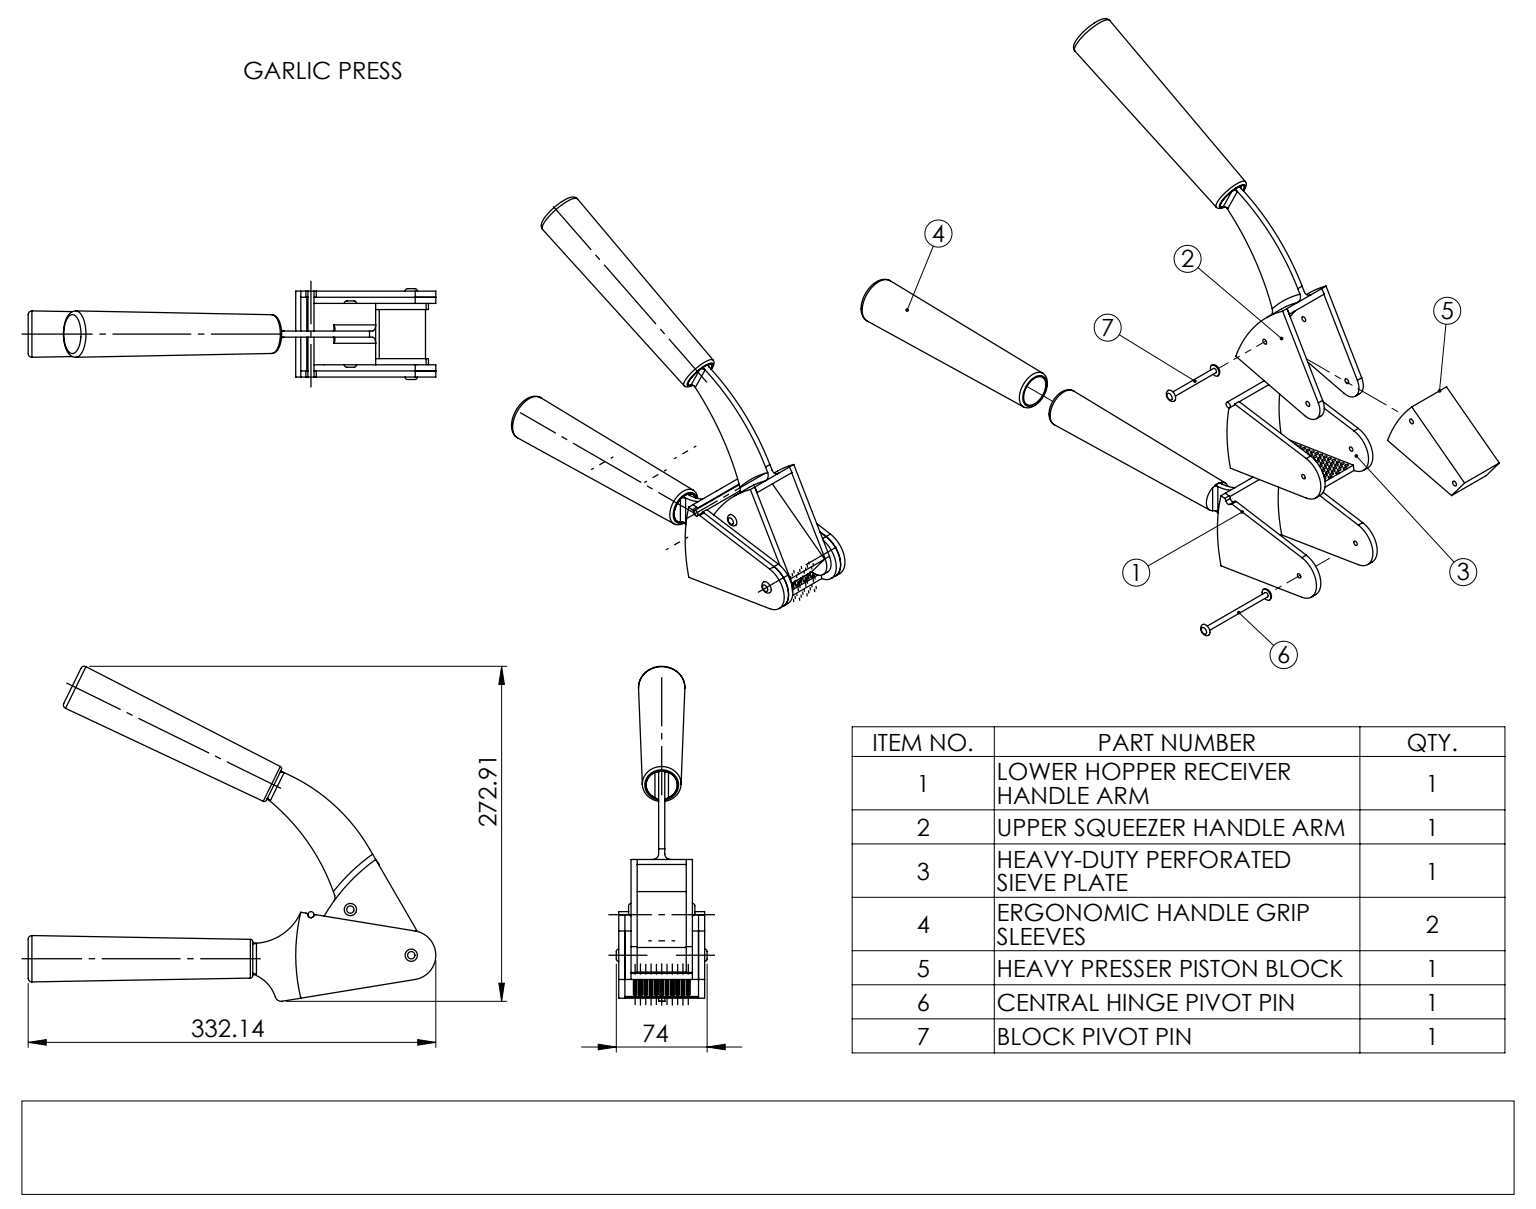
ISO-10303-21;
HEADER;
FILE_DESCRIPTION (('STEP AP214'),
    '1' );
FILE_NAME ('BR-825',
    '2026-10-02T13:02:33',
    ( '' ),
    ( '' ),
    'SwSTEP 2.0',
    'SolidWorks 2026',
    '' );
FILE_SCHEMA (( 'AUTOMOTIVE_DESIGN' ));
ENDSEC;

DATA;
#1 = DIRECTION ( 'NONE',  ( -0.9876526153536341335, -0.1566598588826327021, 0.000000000000000000 ) ) ;
#2 = VERTEX_POINT ( 'NONE', #2570 ) ;
#3 = LINE ( 'NONE', #7217, #14699 ) ;
#4 = ADVANCED_FACE ( 'NONE', ( #13839 ), #888, .F. ) ;
#5 = CARTESIAN_POINT ( 'NONE',  ( -30.20514499443620338, -82.74634522781904877, 4.330127018922213189 ) ) ;
#6 = AXIS2_PLACEMENT_3D ( 'NONE', #420, #4760, #13466 ) ;
#8 = ORIENTED_EDGE ( 'NONE', *, *, #17949, .T. ) ;
#7 = DIRECTION ( 'NONE',  ( 0.000000000000000000, 0.000000000000000000, 1.000000000000000000 ) ) ;
#9 = CIRCLE ( 'NONE', #3911, 1.500000000000000888 ) ;
#10 = ORIENTED_EDGE ( 'NONE', *, *, #1419, .F. ) ;
#11 = CYLINDRICAL_SURFACE ( 'NONE', #12678, 1.500000000000001554 ) ;
#12 = AXIS2_PLACEMENT_3D ( 'NONE', #5144, #6683, #9508 ) ;
#13 = ORIENTED_EDGE ( 'NONE', *, *, #7836, .F. ) ;
#14 = VERTEX_POINT ( 'NONE', #10991 ) ;
#15 = ORIENTED_EDGE ( 'NONE', *, *, #18047, .F. ) ;
#16 = DIRECTION ( 'NONE',  ( -0.1566598588826321192, 0.9876526153536342445, 7.798540720466730171E-17 ) ) ;
#17 = FACE_BOUND ( 'NONE', #10882, .T. ) ;
#18 = AXIS2_PLACEMENT_3D ( 'NONE', #16860, #4970, #18101 ) ;
#19 = EDGE_CURVE ( 'NONE', #12170, #1369, #18158, .T. ) ;
#20 = DIRECTION ( 'NONE',  ( -0.9876526153536341335, -0.1566598588826327021, 0.000000000000000000 ) ) ;
#21 = ORIENTED_EDGE ( 'NONE', *, *, #15181, .F. ) ;
#22 = EDGE_CURVE ( 'NONE', #3591, #12466, #3580, .T. ) ;
#23 = EDGE_CURVE ( 'NONE', #2732, #16279, #9785, .T. ) ;
#24 = EDGE_CURVE ( 'NONE', #1802, #4978, #17849, .T. ) ;
#25 = AXIS2_PLACEMENT_3D ( 'NONE', #11149, #18028, #14009 ) ;
#26 = DIRECTION ( 'NONE',  ( -0.1566598588826321192, 0.9876526153536342445, 7.798540720466730171E-17 ) ) ;
#27 = CARTESIAN_POINT ( 'NONE',  ( -56.41757431148525370, -29.19865005186066043, 17.32050807568881723 ) ) ;
#28 = DIRECTION ( 'NONE',  ( -0.1566598588826321192, 0.9876526153536342445, 7.798540720466730171E-17 ) ) ;
#29 = LINE ( 'NONE', #5530, #5145 ) ;
#30 = FACE_OUTER_BOUND ( 'NONE', #13183, .T. ) ;
#31 = AXIS2_PLACEMENT_3D ( 'NONE', #12240, #913, #6318 ) ;
#32 = DIRECTION ( 'NONE',  ( -0.1566598588826321192, 0.9876526153536342445, 7.798540720466730171E-17 ) ) ;
#33 = ORIENTED_EDGE ( 'NONE', *, *, #662, .F. ) ;
#34 = CIRCLE ( 'NONE', #6695, 1.500000000000000888 ) ;
#35 = ORIENTED_EDGE ( 'NONE', *, *, #7081, .F. ) ;
#36 = EDGE_LOOP ( 'NONE', ( #5022, #14370, #8560, #13804 ) ) ;
#37 = ORIENTED_EDGE ( 'NONE', *, *, #12771, .T. ) ;
#38 = ORIENTED_EDGE ( 'NONE', *, *, #14374, .T. ) ;
#39 = LINE ( 'NONE', #5829, #1016 ) ;
#40 = ORIENTED_EDGE ( 'NONE', *, *, #10473, .T. ) ;
#41 = DIRECTION ( 'NONE',  ( 0.000000000000000000, 0.000000000000000000, 1.000000000000000000 ) ) ;
#42 = AXIS2_PLACEMENT_3D ( 'NONE', #5371, #11127, #3921 ) ;
#43 = CARTESIAN_POINT ( 'NONE',  ( -67.24211807019732134, -88.62108993591773753, 1.443110928631665584E-14 ) ) ;
#44 = VERTEX_POINT ( 'NONE', #12516 ) ;
#45 = AXIS2_PLACEMENT_3D ( 'NONE', #1422, #5499, #1514 ) ;
#46 = CARTESIAN_POINT ( 'NONE',  ( -71.02801022084922522, -26.45362499944938506, 12.99038105676661736 ) ) ;
#47 = APPLICATION_PROTOCOL_DEFINITION ( 'draft international standard', 'automotive_design', 1998, #364 ) ;
#48 = CIRCLE ( 'NONE', #6755, 1.500000000000000000 ) ;
#49 = CARTESIAN_POINT ( 'NONE',  ( 0.000000000000000000, 0.000000000000000000, 32.00000000000000000 ) ) ;
#50 = DIRECTION ( 'NONE',  ( 0.000000000000000000, 0.000000000000000000, 1.000000000000000000 ) ) ;
#51 = EDGE_CURVE ( 'NONE', #10382, #2699, #15096, .T. ) ;
#52 = VECTOR ( 'NONE', #9149, 1000.000000000000000 ) ;
#53 = DIRECTION ( 'NONE',  ( -0.9876526153536336894, -0.1566598588826349503, 0.000000000000000000 ) ) ;
#54 = ORIENTED_EDGE ( 'NONE', *, *, #7944, .T. ) ;
#55 = EDGE_CURVE ( 'NONE', #14250, #12234, #5712, .T. ) ;
#56 = VERTEX_POINT ( 'NONE', #8559 ) ;
#57 = FACE_OUTER_BOUND ( 'NONE', #3238, .T. ) ;
#58 = CARTESIAN_POINT ( 'NONE',  ( -47.32434745236211171, -22.69378838626622397, 1.926565525561698076E-14 ) ) ;
#59 = CIRCLE ( 'NONE', #13963, 20.00000000000001066 ) ;
#60 = CARTESIAN_POINT ( 'NONE',  ( -84.16561914167408531, -33.59999999999994458, -30.00000000000000000 ) ) ;
#61 = CIRCLE ( 'NONE', #8830, 1.500000000000000444 ) ;
#62 = VERTEX_POINT ( 'NONE', #27 ) ;
#63 = LINE ( 'NONE', #14371, #9733 ) ;
#64 = ORIENTED_EDGE ( 'NONE', *, *, #598, .T. ) ;
#65 = AXIS2_PLACEMENT_3D ( 'NONE', #12198, #9374, #18037 ) ;
#66 = VECTOR ( 'NONE', #7491, 1000.000000000000000 ) ;
#67 = DIRECTION ( 'NONE',  ( -0.1566598588826321192, 0.9876526153536342445, 7.798540720466730171E-17 ) ) ;
#68 = CARTESIAN_POINT ( 'NONE',  ( -27.28182215855319015, -24.57718421482303484, -4.330127018922181215 ) ) ;
#69 = DIRECTION ( 'NONE',  ( -0.1566598588826321192, 0.9876526153536342445, 7.798540720466731404E-17 ) ) ;
#70 =( NAMED_UNIT ( * ) SI_UNIT ( $, .STERADIAN. ) SOLID_ANGLE_UNIT ( ) );
#71 = CIRCLE ( 'NONE', #9451, 3.000000000000000000 ) ;
#72 = DIRECTION ( 'NONE',  ( -0.9876526153536336894, -0.1566598588826349503, 0.000000000000000000 ) ) ;
#73 = DIRECTION ( 'NONE',  ( -0.1566598588826321192, 0.9876526153536342445, 7.798540720466731404E-17 ) ) ;
#74 = DIRECTION ( 'NONE',  ( -0.1566598588826321192, 0.9876526153536342445, 7.798540720466730171E-17 ) ) ;
#75 = CYLINDRICAL_SURFACE ( 'NONE', #18095, 1.500000000000001554 ) ;
#76 = EDGE_LOOP ( 'NONE', ( #16554, #5977 ) ) ;
#77 = CARTESIAN_POINT ( 'NONE',  ( -30.53425299135042081, -20.03057078526148516, 8.660254037844417496 ) ) ;
#78 = ADVANCED_FACE ( 'NONE', ( #8643 ), #2771, .F. ) ;
#80 = ORIENTED_EDGE ( 'NONE', *, *, #17512, .T. ) ;
#79 = CARTESIAN_POINT ( 'NONE',  ( -22.79775037928398618, -81.57139628619931671, 17.32050807568881368 ) ) ;
#81 = EDGE_CURVE ( 'NONE', #12067, #4830, #257, .T. ) ;
#82 = DIRECTION ( 'NONE',  ( 0.000000000000000000, 0.000000000000000000, 1.000000000000000000 ) ) ;
#83 = ORIENTED_EDGE ( 'NONE', *, *, #3528, .F. ) ;
#84 = CARTESIAN_POINT ( 'NONE',  ( 0.000000000000000000, 0.000000000000000000, 35.00000000000000000 ) ) ;
#85 = ADVANCED_FACE ( 'NONE', ( #5892 ), #18647, .T. ) ;
#86 = CARTESIAN_POINT ( 'NONE',  ( -89.99999999999998579, -35.00000000000001421, 100.5765140304660861 ) ) ;
#87 =( GEOMETRIC_REPRESENTATION_CONTEXT ( 3 ) GLOBAL_UNCERTAINTY_ASSIGNED_CONTEXT ( ( #8912 ) ) GLOBAL_UNIT_ASSIGNED_CONTEXT ( ( #3872, #4067, #6666 ) ) REPRESENTATION_CONTEXT ( 'NONE', 'WORKASPACE' ) );
#88 = DIRECTION ( 'NONE',  ( -0.000000000000000000, -0.000000000000000000, -1.000000000000000000 ) ) ;
#89 = CYLINDRICAL_SURFACE ( 'NONE', #17046, 1.500000000000001554 ) ;
#90 = DIRECTION ( 'NONE',  ( -0.1566598588826321192, 0.9876526153536342445, 7.798540720466730171E-17 ) ) ;
#91 = CARTESIAN_POINT ( 'NONE',  ( -66.78792677269836986, -30.84357857012828674, 21.65063509461101887 ) ) ;
#92 = CARTESIAN_POINT ( 'NONE',  ( -75.18297400320422241, -32.17518737063066681, 21.65063509461101887 ) ) ;
#93 = VERTEX_POINT ( 'NONE', #10234 ) ;
#94 = DIRECTION ( 'NONE',  ( -0.1566598588826321747, 0.9876526153536343555, 0.000000000000000000 ) ) ;
#95 = DIRECTION ( 'NONE',  ( -0.1566598588826321747, 0.9876526153536343555, 0.000000000000000000 ) ) ;
#96 = CARTESIAN_POINT ( 'NONE',  ( -127.1404785156000941, 9.613695087247878135, -2.500000000000000000 ) ) ;
#97 = ORIENTED_EDGE ( 'NONE', *, *, #2052, .T. ) ;
#98 = VERTEX_POINT ( 'NONE', #12699 ) ;
#99 = CARTESIAN_POINT ( 'NONE',  ( -129.1404785418517918, 9.649298036820672664, 2.500000000000000000 ) ) ;
#100 = AXIS2_PLACEMENT_3D ( 'NONE', #10768, #16585, #15534 ) ;
#101 = EDGE_CURVE ( 'NONE', #13042, #12109, #10138, .T. ) ;
#102 = ORIENTED_EDGE ( 'NONE', *, *, #16935, .T. ) ;
#103 = ORIENTED_EDGE ( 'NONE', *, *, #6276, .F. ) ;
#104 = DIRECTION ( 'NONE',  ( -0.9876526153536336894, -0.1566598588826349503, 0.000000000000000000 ) ) ;
#105 = FACE_BOUND ( 'NONE', #10139, .T. ) ;
#106 = ADVANCED_FACE ( 'NONE', ( #14516 ), #13086, .F. ) ;
#107 = ORIENTED_EDGE ( 'NONE', *, *, #8467, .F. ) ;
#108 = ORIENTED_EDGE ( 'NONE', *, *, #6919, .T. ) ;
#109 =( NAMED_UNIT ( * ) SI_UNIT ( $, .STERADIAN. ) SOLID_ANGLE_UNIT ( ) );
#110 = AXIS2_PLACEMENT_3D ( 'NONE', #4893, #11798, #13415 ) ;
#111 = CARTESIAN_POINT ( 'NONE',  ( 0.000000000000000000, 0.000000000000000000, 35.00000000000000000 ) ) ;
#112 = ORIENTED_EDGE ( 'NONE', *, *, #1667, .T. ) ;
#113 = VERTEX_POINT ( 'NONE', #1359 ) ;
#114 = CARTESIAN_POINT ( 'NONE',  ( -84.16561914167411373, 33.60000000000000142, -30.00000000000000000 ) ) ;
#115 = EDGE_LOOP ( 'NONE', ( #1862, #4295 ) ) ;
#116 = DIRECTION ( 'NONE',  ( -0.9723968097209879646, 0.2333333333333338921, -0.000000000000000000 ) ) ;
#118 = EDGE_CURVE ( 'NONE', #9740, #1864, #12345, .T. ) ;
#117 = LINE ( 'NONE', #3375, #307 ) ;
#119 = FACE_OUTER_BOUND ( 'NONE', #18220, .T. ) ;
#120 = FACE_BOUND ( 'NONE', #14429, .T. ) ;
#121 = DIRECTION ( 'NONE',  ( -0.1566598588826321192, 0.9876526153536342445, 7.798540720466730171E-17 ) ) ;
#122 = EDGE_LOOP ( 'NONE', ( #6243, #4264, #10759 ) ) ;
#123 = EDGE_CURVE ( 'NONE', #15608, #18110, #18554, .T. ) ;
#124 = ORIENTED_EDGE ( 'NONE', *, *, #13553, .F. ) ;
#125 = ORIENTED_EDGE ( 'NONE', *, *, #6218, .F. ) ;
#126 = CARTESIAN_POINT ( 'NONE',  ( -306.1404785418517918, -2.850701963179328668, 9.951701414186818625E-16 ) ) ;
#127 = EDGE_CURVE ( 'NONE', #15127, #18093, #8457, .T. ) ;
#128 = EDGE_CURVE ( 'NONE', #14364, #5884, #10830, .T. ) ;
#129 = ORIENTED_EDGE ( 'NONE', *, *, #2912, .F. ) ;
#130 = FACE_OUTER_BOUND ( 'NONE', #4986, .T. ) ;
#131 = EDGE_CURVE ( 'NONE', #13266, #3195, #7839, .T. ) ;
#132 = CYLINDRICAL_SURFACE ( 'NONE', #16628, 1.500000000000001554 ) ;
#133 = EDGE_LOOP ( 'NONE', ( #5269, #5864 ) ) ;
#134 = EDGE_CURVE ( 'NONE', #306, #3989, #4730, .T. ) ;
#135 = DIRECTION ( 'NONE',  ( -0.9876526153536344665, -0.1566598588826304539, 0.000000000000000000 ) ) ;
#136 = CARTESIAN_POINT ( 'NONE',  ( -54.89646037827696290, -86.66284169988483654, -12.99038105676658539 ) ) ;
#137 = DIRECTION ( 'NONE',  ( -0.1566598588826321192, 0.9876526153536342445, 7.798540720466731404E-17 ) ) ;
#138 = CARTESIAN_POINT ( 'NONE',  ( -48.02252708097939404, -27.86704125135830523, 8.660254037844417496 ) ) ;
#139 = VERTEX_POINT ( 'NONE', #14880 ) ;
#140 = ORIENTED_EDGE ( 'NONE', *, *, #2716, .F. ) ;
#141 = DIRECTION ( 'NONE',  ( -1.000000000000000000, 0.000000000000000000, 0.000000000000000000 ) ) ;
#142 = EDGE_LOOP ( 'NONE', ( #9264, #8766, #6960, #18741, #15276 ) ) ;
#143 = CARTESIAN_POINT ( 'NONE',  ( -35.67686938905902849, -25.90879301532540779, -4.330127018922181215 ) ) ;
#144 = CARTESIAN_POINT ( 'NONE',  ( -24.27922930231443743, -81.80638607452327449, 8.660254037844412167 ) ) ;
#145 = EDGE_CURVE ( 'NONE', #1457, #13070, #13868, .T. ) ;
#146 = ORIENTED_EDGE ( 'NONE', *, *, #12497, .F. ) ;
#147 = DIRECTION ( 'NONE',  ( -0.1566598588826321747, 0.9876526153536343555, 0.000000000000000000 ) ) ;
#148 = EDGE_CURVE ( 'NONE', #7107, #5722, #1632, .T. ) ;
#149 = EDGE_CURVE ( 'NONE', #14051, #4382, #6373, .T. ) ;
#150 = EDGE_CURVE ( 'NONE', #1792, #949, #14691, .T. ) ;
#151 = DIRECTION ( 'NONE',  ( -0.1566598588826321192, 0.9876526153536342445, 7.798540720466730171E-17 ) ) ;
#152 = TOROIDAL_SURFACE ( 'NONE', #18040, 3.000000000000004441, 2.000000000000000000 ) ;
#153 = LINE ( 'NONE', #5658, #5168 ) ;
#154 = CARTESIAN_POINT ( 'NONE',  ( -70.24471092643608472, -31.39188807621751209, 21.65063509461101887 ) ) ;
#155 = SHAPE_REPRESENTATION_RELATIONSHIP ( 'NONE' , 'NONE' ,  #6739, #1868 ) ;
#156 = EDGE_LOOP ( 'NONE', ( #2014, #11521, #8711, #17506 ) ) ;
#157 = CARTESIAN_POINT ( 'NONE',  ( -33.00338452973448966, -20.42222043246806251, 4.330127018922218518 ) ) ;
#158 = DIRECTION ( 'NONE',  ( -0.1566598588826321192, 0.9876526153536342445, 7.798540720466730171E-17 ) ) ;
#159 = DIRECTION ( 'NONE',  ( -0.1566598588826321192, 0.9876526153536342445, 7.798540720466730171E-17 ) ) ;
#160 = CARTESIAN_POINT ( 'NONE',  ( -18.35331361019266794, -80.86642692122747178, 4.330127018922213189 ) ) ;
#161 = ORIENTED_EDGE ( 'NONE', *, *, #2086, .F. ) ;
#162 = FACE_OUTER_BOUND ( 'NONE', #5968, .T. ) ;
#164 = ORIENTED_EDGE ( 'NONE', *, *, #5902, .T. ) ;
#163 = CARTESIAN_POINT ( 'NONE',  ( -6.047290928450125946, -21.20899724884646531, -21.65063509461098334 ) ) ;
#165 = CIRCLE ( 'NONE', #14403, 12.74754878398197633 ) ;
#166 = CARTESIAN_POINT ( 'NONE',  ( -39.91695283720987675, -21.51883944464648479, -4.330127018922180326 ) ) ;
#167 = EDGE_LOOP ( 'NONE', ( #17757, #5769 ) ) ;
#168 = CARTESIAN_POINT ( 'NONE',  ( -16.91146969734005268, -22.93225569655540141, -8.660254037844380193 ) ) ;
#169 = EDGE_CURVE ( 'NONE', #4575, #3501, #2377, .T. ) ;
#170 = DIRECTION ( 'NONE',  ( -0.9876526153536336894, -0.1566598588826349503, 0.000000000000000000 ) ) ;
#171 = FACE_OUTER_BOUND ( 'NONE', #4320, .T. ) ;
#172 = DIRECTION ( 'NONE',  ( -0.1566598588826321192, 0.9876526153536342445, 7.798540720466730171E-17 ) ) ;
#173 = CARTESIAN_POINT ( 'NONE',  ( -58.88670584986932255, -29.59029969906724133, 12.99038105676661736 ) ) ;
#174 = EDGE_CURVE ( 'NONE', #9818, #7902, #192, .T. ) ;
#175 = LINE ( 'NONE', #6157, #13878 ) ;
#176 = AXIS2_PLACEMENT_3D ( 'NONE', #2016, #3423, #9416 ) ;
#177 = ORIENTED_EDGE ( 'NONE', *, *, #17607, .F. ) ;
#178 = CARTESIAN_POINT ( 'NONE',  ( -22.79775037928398618, -81.57139628619930249, -17.32050807568878525 ) ) ;
#179 = CARTESIAN_POINT ( 'NONE',  ( -34.19539046602857724, -25.67380322700145356, 12.99038105676661736 ) ) ;
#180 = ORIENTED_EDGE ( 'NONE', *, *, #16256, .T. ) ;
#181 = ORIENTED_EDGE ( 'NONE', *, *, #3310, .F. ) ;
#182 = CARTESIAN_POINT ( 'NONE',  ( -60.36818477289978091, -29.82528948739120267, -12.99038105676658006 ) ) ;
#183 = CIRCLE ( 'NONE', #2605, 1.500000000000000888 ) ;
#184 = ORIENTED_EDGE ( 'NONE', *, *, #555, .T. ) ;
#185 = ORIENTED_EDGE ( 'NONE', *, *, #890, .F. ) ;
#186 = CARTESIAN_POINT ( 'NONE',  ( -68.55887868246516348, -26.06197535224280770, 17.32050807568882078 ) ) ;
#187 = CARTESIAN_POINT ( 'NONE',  ( -37.94164760650264867, -21.20551972688121012, -21.65063509461098334 ) ) ;
#188 = EDGE_LOOP ( 'NONE', ( #13607, #15627 ) ) ;
#189 = CARTESIAN_POINT ( 'NONE',  ( -49.01017969633304006, -28.02370111024093191, -12.99038105676658006 ) ) ;
#190 = CIRCLE ( 'NONE', #802, 42.89102435249441925 ) ;
#191 = EDGE_CURVE ( 'NONE', #13070, #8810, #6083, .T. ) ;
#192 = LINE ( 'NONE', #17673, #12969 ) ;
#193 = EDGE_LOOP ( 'NONE', ( #12370, #7151, #5297, #6845 ) ) ;
#194 =( NAMED_UNIT ( * ) PLANE_ANGLE_UNIT ( ) SI_UNIT ( $, .RADIAN. ) );
#195 = ORIENTED_EDGE ( 'NONE', *, *, #18603, .T. ) ;
#196 = CARTESIAN_POINT ( 'NONE',  ( -64.20000000000000284, 2.694222958124180951E-16, -25.00000000000000000 ) ) ;
#197 = AXIS2_PLACEMENT_3D ( 'NONE', #13789, #13899, #10956 ) ;
#199 = EDGE_CURVE ( 'NONE', #827, #16818, #10252, .T. ) ;
#198 = DIRECTION ( 'NONE',  ( 1.000000000000000000, 0.000000000000000000, -0.000000000000000000 ) ) ;
#200 = DIRECTION ( 'NONE',  ( -0.1566598588826321192, 0.9876526153536342445, 7.798540720466731404E-17 ) ) ;
#201 = ADVANCED_FACE ( 'NONE', ( #1648 ), #132, .F. ) ;
#202 = VERTEX_POINT ( 'NONE', #5909 ) ;
#203 = ORIENTED_EDGE ( 'NONE', *, *, #2611, .T. ) ;
#204 = ORIENTED_EDGE ( 'NONE', *, *, #16861, .F. ) ;
#205 = ORIENTED_EDGE ( 'NONE', *, *, #601, .T. ) ;
#206 = DIRECTION ( 'NONE',  ( -0.1566598588826321192, 0.9876526153536342445, 7.798540720466731404E-17 ) ) ;
#207 = AXIS2_PLACEMENT_3D ( 'NONE', #17977, #18347, #1736 ) ;
#208 = ORIENTED_EDGE ( 'NONE', *, *, #14608, .T. ) ;
#209 = FACE_BOUND ( 'NONE', #76, .T. ) ;
#210 = CARTESIAN_POINT ( 'NONE',  ( 10.28861223506262412, -76.32329101363113466, 8.660254037844406838 ) ) ;
#211 = VERTEX_POINT ( 'NONE', #5994 ) ;
#212 = PRESENTATION_LAYER_ASSIGNMENT (  '', '', ( #11387 ) ) ;
#213 = EDGE_LOOP ( 'NONE', ( #813, #9222, #12211, #16308 ) ) ;
#214 = CIRCLE ( 'NONE', #11085, 1.500000000000000888 ) ;
#215 = EDGE_LOOP ( 'NONE', ( #10832, #6172, #11697, #10724 ) ) ;
#216 = CIRCLE ( 'NONE', #4738, 1.500000000000000444 ) ;
#217 = DIRECTION ( 'NONE',  ( -0.9876526153536344665, -0.1566598588826304539, 0.000000000000000000 ) ) ;
#218 = CIRCLE ( 'NONE', #4461, 1.499999999999999556 ) ;
#219 = EDGE_CURVE ( 'NONE', #16637, #6756, #7426, .T. ) ;
#220 = EDGE_CURVE ( 'NONE', #5802, #9058, #10861, .T. ) ;
#221 = CARTESIAN_POINT ( 'NONE',  ( -18.39294862037050393, -23.16724548487935564, 1.869203119972154228E-14 ) ) ;
#222 = CARTESIAN_POINT ( 'NONE',  ( -10.98555400521827607, -21.99229654325962002, 12.99038105676661381 ) ) ;
#224 = EDGE_CURVE ( 'NONE', #15083, #7553, #10560, .T. ) ;
#223 = DIRECTION ( 'NONE',  ( -0.000000000000000000, -0.000000000000000000, -1.000000000000000000 ) ) ;
#225 = FACE_OUTER_BOUND ( 'NONE', #16348, .T. ) ;
#226 = ORIENTED_EDGE ( 'NONE', *, *, #15016, .F. ) ;
#227 = VERTEX_POINT ( 'NONE', #8930 ) ;
#228 = CARTESIAN_POINT ( 'NONE',  ( -19.34096622554629263, -81.02308678011010556, 1.424741226644455312E-14 ) ) ;
#229 = ORIENTED_EDGE ( 'NONE', *, *, #5595, .F. ) ;
#230 = CIRCLE ( 'NONE', #18445, 2.199999999999993516 ) ;
#231 = LINE ( 'NONE', #17611, #15362 ) ;
#232 = ORIENTED_EDGE ( 'NONE', *, *, #13411, .F. ) ;
#233 = ORIENTED_EDGE ( 'NONE', *, *, #9764, .F. ) ;
#234 = ORIENTED_EDGE ( 'NONE', *, *, #16412, .F. ) ;
#235 = CARTESIAN_POINT ( 'NONE',  ( -9.299721761247353058, -16.66238381928489787, -17.32050807568878170 ) ) ;
#236 = FACE_BOUND ( 'NONE', #6125, .T. ) ;
#237 = LINE ( 'NONE', #7306, #7511 ) ;
#238 = CARTESIAN_POINT ( 'NONE',  ( -64.77298653181324539, -88.22944028871116018, 21.65063509461101532 ) ) ;
#239 = EDGE_CURVE ( 'NONE', #10470, #12526, #9677, .T. ) ;
#240 = CIRCLE ( 'NONE', #6612, 1.500000000000000444 ) ;
#241 = VERTEX_POINT ( 'NONE', #17685 ) ;
#242 = EDGE_CURVE ( 'NONE', #4960, #1643, #5109, .T. ) ;
#243 = DIRECTION ( 'NONE',  ( -0.9876526153536336894, -0.1566598588826349503, 0.000000000000000000 ) ) ;
#244 = CARTESIAN_POINT ( 'NONE',  ( -14.40270314877813895, -80.23978748569693664, -17.32050807568878525 ) ) ;
#245 = CARTESIAN_POINT ( 'NONE',  ( -129.1404785418517918, 8.649298036820676217, 5.500000000000000000 ) ) ;
#246 = CYLINDRICAL_SURFACE ( 'NONE', #528, 2.000000000000001776 ) ;
#247 = EDGE_LOOP ( 'NONE', ( #10607, #2910 ) ) ;
#248 = EDGE_LOOP ( 'NONE', ( #11901, #15407, #18357, #803 ) ) ;
#249 = CARTESIAN_POINT ( 'NONE',  ( -41.39843176024032800, -21.75382923297043192, 4.330127018922218518 ) ) ;
#250 = CIRCLE ( 'NONE', #2017, 1.500000000000000444 ) ;
#251 = AXIS2_PLACEMENT_3D ( 'NONE', #14278, #17128, #4490 ) ;
#252 = ORIENTED_EDGE ( 'NONE', *, *, #3818, .T. ) ;
#253 = VECTOR ( 'NONE', #1467, 1000.000000000000000 ) ;
#254 = EDGE_LOOP ( 'NONE', ( #5319, #8500, #14701, #2198 ) ) ;
#255 = ORIENTED_EDGE ( 'NONE', *, *, #6970, .T. ) ;
#256 = DIRECTION ( 'NONE',  ( 0.000000000000000000, 0.000000000000000000, 1.000000000000000000 ) ) ;
#257 = CIRCLE ( 'NONE', #7250, 1.499999999999999556 ) ;
#258 = LINE ( 'NONE', #13329, #11510 ) ;
#259 = DIRECTION ( 'NONE',  ( 1.000000000000000000, 0.000000000000000000, -0.000000000000000000 ) ) ;
#260 = AXIS2_PLACEMENT_3D ( 'NONE', #1453, #14527, #297 ) ;
#261 = CARTESIAN_POINT ( 'NONE',  ( -36.62488699423482785, -83.76463431055616127, -21.65063509461098690 ) ) ;
#262 = CARTESIAN_POINT ( 'NONE',  ( -41.39843176024032800, -21.75382923297042836, -4.330127018922180326 ) ) ;
#263 = CIRCLE ( 'NONE', #6336, 2.200000000000000178 ) ;
#264 = DIRECTION ( 'NONE',  ( -0.9876526153536336894, -0.1566598588826349503, 0.000000000000000000 ) ) ;
#265 = CARTESIAN_POINT ( 'NONE',  ( -26.78799585087635649, -24.49885428538171794, -8.660254037844380193 ) ) ;
#266 = FACE_OUTER_BOUND ( 'NONE', #3188, .T. ) ;
#267 = ORIENTED_EDGE ( 'NONE', *, *, #13623, .F. ) ;
#269 = EDGE_LOOP ( 'NONE', ( #9815, #12862, #15948, #5626 ) ) ;
#268 = DIRECTION ( 'NONE',  ( -0.9876526153536336894, -0.1566598588826349503, 0.000000000000000000 ) ) ;
#270 = EDGE_CURVE ( 'NONE', #17286, #16790, #6357, .T. ) ;
#271 = AXIS2_PLACEMENT_3D ( 'NONE', #15102, #6588, #11007 ) ;
#272 = VERTEX_POINT ( 'NONE', #11653 ) ;
#273 = EDGE_CURVE ( 'NONE', #17252, #3975, #18174, .T. ) ;
#274 = CARTESIAN_POINT ( 'NONE',  ( -6.047290928450125946, -21.20899724884646531, 21.65063509461101177 ) ) ;
#275 = VECTOR ( 'NONE', #8347, 1000.000000000000000 ) ;
#276 = ORIENTED_EDGE ( 'NONE', *, *, #13888, .T. ) ;
#277 = ORIENTED_EDGE ( 'NONE', *, *, #10855, .F. ) ;
#278 = FACE_OUTER_BOUND ( 'NONE', #17914, .T. ) ;
#279 = CIRCLE ( 'NONE', #11460, 1.500000000000000444 ) ;
#280 = EDGE_CURVE ( 'NONE', #14450, #6414, #16167, .T. ) ;
#281 = VECTOR ( 'NONE', #15110, 1000.000000000000000 ) ;
#282 = CIRCLE ( 'NONE', #10852, 1.500000000000000000 ) ;
#283 = DIRECTION ( 'NONE',  ( -0.9876526153536341335, -0.1566598588826327021, 0.000000000000000000 ) ) ;
#284 = CARTESIAN_POINT ( 'NONE',  ( 2.000000000000000000, 0.000000000000000000, 30.00000000000000000 ) ) ;
#285 = CARTESIAN_POINT ( 'NONE',  ( -13.25033222266188560, -17.28902325481542235, 4.330127018922214965 ) ) ;
#286 = AXIS2_PLACEMENT_3D ( 'NONE', #9882, #15657, #10154 ) ;
#287 = AXIS2_PLACEMENT_3D ( 'NONE', #9251, #13887, #9450 ) ;
#288 = DIRECTION ( 'NONE',  ( 0.9826218788918642533, 0.1856185419698762884, -0.000000000000000000 ) ) ;
#289 = AXIS2_PLACEMENT_3D ( 'NONE', #791, #6676, #10995 ) ;
#290 = ORIENTED_EDGE ( 'NONE', *, *, #11265, .T. ) ;
#291 = FACE_BOUND ( 'NONE', #9868, .T. ) ;
#292 = AXIS2_PLACEMENT_3D ( 'NONE', #3529, #12534, #16843 ) ;
#293 = DIRECTION ( 'NONE',  ( -1.000000000000000000, 0.000000000000000000, 0.000000000000000000 ) ) ;
#294 = VERTEX_POINT ( 'NONE', #7445 ) ;
#295 = DIRECTION ( 'NONE',  ( -0.9876526153536341335, -0.1566598588826327021, 0.000000000000000000 ) ) ;
#296 = VECTOR ( 'NONE', #9069, 1000.000000000000000 ) ;
#297 = DIRECTION ( 'NONE',  ( 0.000000000000000000, 0.000000000000000000, 1.000000000000000000 ) ) ;
#298 = ORIENTED_EDGE ( 'NONE', *, *, #1505, .F. ) ;
#299 = VERTEX_POINT ( 'NONE', #6020 ) ;
#300 = ORIENTED_EDGE ( 'NONE', *, *, #13362, .F. ) ;
#301 = AXIS2_PLACEMENT_3D ( 'NONE', #1034, #11223, #5560 ) ;
#302 = ORIENTED_EDGE ( 'NONE', *, *, #6850, .F. ) ;
#303 = DIRECTION ( 'NONE',  ( -0.9876526153536336894, -0.1566598588826349503, 0.000000000000000000 ) ) ;
#304 = EDGE_CURVE ( 'NONE', #7962, #8290, #17617, .T. ) ;
#305 = ORIENTED_EDGE ( 'NONE', *, *, #9387, .T. ) ;
#306 = VERTEX_POINT ( 'NONE', #6126 ) ;
#307 = VECTOR ( 'NONE', #16481, 1000.000000000000000 ) ;
#308 = FACE_BOUND ( 'NONE', #13049, .T. ) ;
#309 = DIRECTION ( 'NONE',  ( -0.9876526153536336894, -0.1566598588826349503, 0.000000000000000000 ) ) ;
#310 = VECTOR ( 'NONE', #14810, 1000.000000000000000 ) ;
#311 = VERTEX_POINT ( 'NONE', #14829 ) ;
#312 = CARTESIAN_POINT ( 'NONE',  ( -23.33121169713865584, -23.95054477929251036, -8.660254037844380193 ) ) ;
#313 = VECTOR ( 'NONE', #867, 1000.000000000000000 ) ;
#314 = EDGE_LOOP ( 'NONE', ( #6630, #11469 ) ) ;
#315 = EDGE_CURVE ( 'NONE', #5884, #5893, #1848, .T. ) ;
#316 = EDGE_CURVE ( 'NONE', #12986, #12973, #2391, .T. ) ;
#317 = EDGE_LOOP ( 'NONE', ( #16039, #7700, #562, #13733 ) ) ;
#318 = AXIS2_PLACEMENT_3D ( 'NONE', #5866, #8616, #8694 ) ;
#319 = DIRECTION ( 'NONE',  ( 0.000000000000000000, 0.000000000000000000, 1.000000000000000000 ) ) ;
#320 = DIRECTION ( 'NONE',  ( -0.1566598588826321192, 0.9876526153536342445, 7.798540720466730171E-17 ) ) ;
#322 = CARTESIAN_POINT ( 'NONE',  ( -13.45468554360235203, -22.38394619046619383, 1.869203119972154228E-14 ) ) ;
#321 = AXIS2_PLACEMENT_3D ( 'NONE', #1598, #12854, #13040 ) ;
#323 = DIRECTION ( 'NONE',  ( -0.1566598588826321192, 0.9876526153536342445, 7.798540720466731404E-17 ) ) ;
#324 = CARTESIAN_POINT ( 'NONE',  ( -6.995308533625909320, -79.06483854407721878, 21.65063509461100821 ) ) ;
#325 = LINE ( 'NONE', #9139, #5689 ) ;
#326 = ORIENTED_EDGE ( 'NONE', *, *, #13082, .F. ) ;
#327 = ORIENTED_EDGE ( 'NONE', *, *, #12450, .F. ) ;
#328 = LINE ( 'NONE', #4668, #9322 ) ;
#329 = AXIS2_PLACEMENT_3D ( 'NONE', #4692, #16469, #16269 ) ;
#330 = DIRECTION ( 'NONE',  ( -0.1566598588826321192, 0.9876526153536342445, 7.798540720466730171E-17 ) ) ;
#331 = DIRECTION ( 'NONE',  ( -0.1566598588826321192, 0.9876526153536342445, 7.798540720466730171E-17 ) ) ;
#332 = CIRCLE ( 'NONE', #3341, 1.500000000000000888 ) ;
#333 = ADVANCED_FACE ( 'NONE', ( #10729 ), #15383, .F. ) ;
#334 = VERTEX_POINT ( 'NONE', #16930 ) ;
#335 = CARTESIAN_POINT ( 'NONE',  ( -75.18297400320422241, -32.17518737063066681, 21.65063509461101887 ) ) ;
#336 = CIRCLE ( 'NONE', #16374, 1.500000000000000888 ) ;
#338 = FACE_BOUND ( 'NONE', #5848, .T. ) ;
#337 = AXIS2_PLACEMENT_3D ( 'NONE', #9442, #15216, #13774 ) ;
#339 = EDGE_CURVE ( 'NONE', #7418, #9571, #3618, .T. ) ;
#340 = DIRECTION ( 'NONE',  ( 0.000000000000000000, 0.000000000000000000, 1.000000000000000000 ) ) ;
#341 = CIRCLE ( 'NONE', #12123, 1.500000000000001332 ) ;
#342 = DIRECTION ( 'NONE',  ( -0.1566598588826321192, 0.9876526153536342445, 7.798540720466731404E-17 ) ) ;
#343 = DIRECTION ( 'NONE',  ( -0.1566598588826321192, 0.9876526153536342445, 7.798540720466730171E-17 ) ) ;
#344 = VERTEX_POINT ( 'NONE', #5255 ) ;
#345 = DIRECTION ( 'NONE',  ( -0.1566598588826321747, 0.9876526153536343555, 0.000000000000000000 ) ) ;
#346 = CARTESIAN_POINT ( 'NONE',  ( -45.34904222165486942, -22.38046866850094929, -17.32050807568878170 ) ) ;
#347 = AXIS2_PLACEMENT_3D ( 'NONE', #6635, #963, #6737 ) ;
#348 = VECTOR ( 'NONE', #6882, 1000.000000000000000 ) ;
#349 = FACE_OUTER_BOUND ( 'NONE', #8068, .T. ) ;
#350 = LINE ( 'NONE', #15811, #2031 ) ;
#351 = EDGE_LOOP ( 'NONE', ( #7291, #2729, #13644, #16148 ) ) ;
#352 = CARTESIAN_POINT ( 'NONE',  ( -45.01993422474065198, -85.09624311105852712, 4.330127018922213189 ) ) ;
#353 = EDGE_CURVE ( 'NONE', #8550, #12053, #18503, .T. ) ;
#354 = ORIENTED_EDGE ( 'NONE', *, *, #5419, .T. ) ;
#355 = CIRCLE ( 'NONE', #13059, 2.000000000000000000 ) ;
#356 = VERTEX_POINT ( 'NONE', #16529 ) ;
#357 = EDGE_CURVE ( 'NONE', #4379, #18393, #1509, .T. ) ;
#358 = EDGE_CURVE ( 'NONE', #1477, #15259, #8155, .T. ) ;
#359 = EDGE_CURVE ( 'NONE', #9050, #9141, #4270, .T. ) ;
#360 = EDGE_LOOP ( 'NONE', ( #2874, #17765 ) ) ;
#361 = DIRECTION ( 'NONE',  ( 0.000000000000000000, 0.000000000000000000, 1.000000000000000000 ) ) ;
#362 = EDGE_CURVE ( 'NONE', #1820, #10566, #9051, .T. ) ;
#363 = AXIS2_PLACEMENT_3D ( 'NONE', #14211, #2358, #12673 ) ;
#364 = APPLICATION_CONTEXT ( 'automotive_design' ) ;
#365 = DIRECTION ( 'NONE',  ( -0.1566598588826321192, 0.9876526153536342445, 7.798540720466730171E-17 ) ) ;
#366 = ORIENTED_EDGE ( 'NONE', *, *, #8931, .T. ) ;
#367 = CARTESIAN_POINT ( 'NONE',  ( -48.80582637539254875, -22.92877817459017464, 17.32050807568882078 ) ) ;
#368 = CARTESIAN_POINT ( 'NONE',  ( -66.25446545484369665, -88.46443007703511796, -12.99038105676658539 ) ) ;
#369 = DIRECTION ( 'NONE',  ( -0.9876526153536336894, -0.1566598588826349503, 0.000000000000000000 ) ) ;
#370 = VERTEX_POINT ( 'NONE', #11385 ) ;
#371 = AXIS2_PLACEMENT_3D ( 'NONE', #10848, #743, #7570 ) ;
#372 = CARTESIAN_POINT ( 'NONE',  ( -46.50141314777110324, -85.33123289938248490, 4.330127018922213189 ) ) ;
#373 = ORIENTED_EDGE ( 'NONE', *, *, #11541, .F. ) ;
#374 = DIRECTION ( 'NONE',  ( 1.000000000000000000, 0.000000000000000000, 0.000000000000000000 ) ) ;
#375 = AXIS2_PLACEMENT_3D ( 'NONE', #5395, #11058, #12194 ) ;
#376 = DIRECTION ( 'NONE',  ( -0.9876526153536341335, -0.1566598588826327021, 0.000000000000000000 ) ) ;
#377 = EDGE_LOOP ( 'NONE', ( #5700, #15642 ) ) ;
#379 = ORIENTED_EDGE ( 'NONE', *, *, #9515, .T. ) ;
#378 = DIRECTION ( 'NONE',  ( -0.9876526153536341335, -0.1566598588826327021, 0.000000000000000000 ) ) ;
#380 = CIRCLE ( 'NONE', #16419, 13.78215425775057668 ) ;
#381 = ORIENTED_EDGE ( 'NONE', *, *, #387, .F. ) ;
#382 = DIRECTION ( 'NONE',  ( 0.000000000000000000, 0.000000000000000000, 1.000000000000000000 ) ) ;
#383 = ORIENTED_EDGE ( 'NONE', *, *, #18100, .F. ) ;
#384 = VERTEX_POINT ( 'NONE', #4086 ) ;
#385 = EDGE_LOOP ( 'NONE', ( #16397, #10275 ) ) ;
#386 = DIRECTION ( 'NONE',  ( -0.9876526153536341335, -0.1566598588826327021, 0.000000000000000000 ) ) ;
#387 = EDGE_CURVE ( 'NONE', #11399, #16710, #13584, .T. ) ;
#388 = STYLED_ITEM ( 'NONE', ( #17094 ), #8708 ) ;
#389 = ORIENTED_EDGE ( 'NONE', *, *, #13835, .T. ) ;
#390 = CARTESIAN_POINT ( 'NONE',  ( -48.97054468615517919, -85.72288254658904805, 8.660254037844412167 ) ) ;
#391 = ORIENTED_EDGE ( 'NONE', *, *, #358, .T. ) ;
#392 = CYLINDRICAL_SURFACE ( 'NONE', #15221, 1.500000000000001554 ) ;
#393 = ORIENTED_EDGE ( 'NONE', *, *, #4749, .F. ) ;
#394 = EDGE_CURVE ( 'NONE', #17063, #537, #14514, .T. ) ;
#395 = LINE ( 'NONE', #17952, #3848 ) ;
#396 = ORIENTED_EDGE ( 'NONE', *, *, #516, .F. ) ;
#397 = ORIENTED_EDGE ( 'NONE', *, *, #14939, .F. ) ;
#398 = AXIS2_PLACEMENT_3D ( 'NONE', #6831, #12574, #2548 ) ;
#399 = DIRECTION ( 'NONE',  ( -0.9876526153536336894, -0.1566598588826350336, 0.000000000000000000 ) ) ;
#400 = FACE_OUTER_BOUND ( 'NONE', #2830, .T. ) ;
#401 = ORIENTED_EDGE ( 'NONE', *, *, #13050, .T. ) ;
#402 = ORIENTED_EDGE ( 'NONE', *, *, #11892, .F. ) ;
#403 = VERTEX_POINT ( 'NONE', #17028 ) ;
#404 = ORIENTED_EDGE ( 'NONE', *, *, #8014, .T. ) ;
#405 = VERTEX_POINT ( 'NONE', #2589 ) ;
#406 = ORIENTED_EDGE ( 'NONE', *, *, #492, .F. ) ;
#407 = CARTESIAN_POINT ( 'NONE',  ( -21.81009776393036503, -81.41473642731666871, -21.65063509461098690 ) ) ;
#408 = ORIENTED_EDGE ( 'NONE', *, *, #6164, .F. ) ;
#409 = ORIENTED_EDGE ( 'NONE', *, *, #15155, .F. ) ;
#410 = FACE_BOUND ( 'NONE', #1885, .T. ) ;
#411 = VERTEX_POINT ( 'NONE', #18575 ) ;
#412 = CARTESIAN_POINT ( 'NONE',  ( -44.03228160938703439, -84.93958325217590755, 8.660254037844412167 ) ) ;
#413 = ORIENTED_EDGE ( 'NONE', *, *, #12861, .T. ) ;
#414 = ADVANCED_FACE ( 'NONE', ( #17211 ), #2684, .T. ) ;
#415 = ORIENTED_EDGE ( 'NONE', *, *, #13647, .F. ) ;
#416 = FACE_BOUND ( 'NONE', #8311, .T. ) ;
#417 = DIRECTION ( 'NONE',  ( 1.000000000000000000, 0.000000000000000000, 0.000000000000000000 ) ) ;
#418 = ADVANCED_FACE ( 'NONE', ( #10070 ), #1375, .F. ) ;
#419 = CARTESIAN_POINT ( 'NONE',  ( -46.50141314777111745, -85.33123289938247069, -21.65063509461098690 ) ) ;
#420 = CARTESIAN_POINT ( 'NONE',  ( -75.18297400320422241, -32.17518737063066681, 4.330127018922217630 ) ) ;
#421 = PLANE ( 'NONE',  #6625 ) ;
#422 = DIRECTION ( 'NONE',  ( -0.1566598588826321192, 0.9876526153536342445, 7.798540720466731404E-17 ) ) ;
#423 = DIRECTION ( 'NONE',  ( -0.9876526153536336894, -0.1566598588826349503, 0.000000000000000000 ) ) ;
#424 = ORIENTED_EDGE ( 'NONE', *, *, #224, .F. ) ;
#425 = EDGE_LOOP ( 'NONE', ( #6614, #11556 ) ) ;
#426 = TOROIDAL_SURFACE ( 'NONE', #13412, 155.0000000000000284, 5.000000000000000000 ) ;
#427 = CARTESIAN_POINT ( 'NONE',  ( -51.97313754239394257, -28.49368068688882971, -21.65063509461098334 ) ) ;
#428 = DIRECTION ( 'NONE',  ( -0.1566598588826321192, 0.9876526153536342445, 7.798540720466730171E-17 ) ) ;
#429 = ORIENTED_EDGE ( 'NONE', *, *, #3774, .F. ) ;
#430 = CARTESIAN_POINT ( 'NONE',  ( -349.0394899966146909, 23.59157312255261729, 2.567204941047426911E-15 ) ) ;
#431 = DIRECTION ( 'NONE',  ( -0.1566598588826321192, 0.9876526153536342445, 7.798540720466730171E-17 ) ) ;
#432 = DIRECTION ( 'NONE',  ( -0.1566598588826321192, 0.9876526153536342445, 7.798540720466731404E-17 ) ) ;
#433 = FACE_OUTER_BOUND ( 'NONE', #8720, .T. ) ;
#434 = EDGE_CURVE ( 'NONE', #14223, #211, #7251, .T. ) ;
#435 = CARTESIAN_POINT ( 'NONE',  ( -1.109027851681966492, -20.42569795443330349, 12.99038105676661026 ) ) ;
#436 = FACE_OUTER_BOUND ( 'NONE', #14679, .T. ) ;
#437 = CARTESIAN_POINT ( 'NONE',  ( -38.10636591726525069, -83.99962409888011905, 21.65063509461101532 ) ) ;
#438 = DIRECTION ( 'NONE',  ( 1.000000000000000000, 0.000000000000000000, 0.000000000000000000 ) ) ;
#439 = ORIENTED_EDGE ( 'NONE', *, *, #9830, .F. ) ;
#440 = ORIENTED_EDGE ( 'NONE', *, *, #10556, .F. ) ;
#441 = DIRECTION ( 'NONE',  ( -0.1566598588826321192, 0.9876526153536342445, 7.798540720466730171E-17 ) ) ;
#442 = VERTEX_POINT ( 'NONE', #9802 ) ;
#443 = ORIENTED_EDGE ( 'NONE', *, *, #4057, .T. ) ;
#444 = EDGE_CURVE ( 'NONE', #18320, #13724, #15774, .T. ) ;
#445 = ORIENTED_EDGE ( 'NONE', *, *, #17707, .F. ) ;
#446 = CIRCLE ( 'NONE', #10419, 1.500000000000000444 ) ;
#447 = DIRECTION ( 'NONE',  ( 0.000000000000000000, 0.000000000000000000, -1.000000000000000000 ) ) ;
#448 = ORIENTED_EDGE ( 'NONE', *, *, #11230, .F. ) ;
#449 = DIRECTION ( 'NONE',  ( -0.1566598588826321192, 0.9876526153536342445, 7.798540720466730171E-17 ) ) ;
#450 = VERTEX_POINT ( 'NONE', #8374 ) ;
#451 = DIRECTION ( 'NONE',  ( -0.1566598588826321747, 0.9876526153536343555, 0.000000000000000000 ) ) ;
#452 = DIRECTION ( 'NONE',  ( -0.1566598588826321747, 0.9876526153536343555, 0.000000000000000000 ) ) ;
#453 = DIRECTION ( 'NONE',  ( -0.9876526153536341335, -0.1566598588826327021, 0.000000000000000000 ) ) ;
#454 = PRODUCT ( 'Central Hinge Pivot Pin', 'Central Hinge Pivot Pin', '', ( #9983 ) ) ;
#455 = CARTESIAN_POINT ( 'NONE',  ( -37.61253960958843834, -83.92129416943879505, 1.443110928631665584E-14 ) ) ;
#456 = ORIENTED_EDGE ( 'NONE', *, *, #5446, .T. ) ;
#457 = FACE_OUTER_BOUND ( 'NONE', #12580, .T. ) ;
#458 = FACE_BOUND ( 'NONE', #12232, .T. ) ;
#459 = ADVANCED_FACE ( 'NONE', ( #14152 ), #2791, .F. ) ;
#460 = DIRECTION ( 'NONE',  ( -0.1566598588826321192, 0.9876526153536342445, 7.798540720466730171E-17 ) ) ;
#461 = ORIENTED_EDGE ( 'NONE', *, *, #12663, .T. ) ;
#462 = DIRECTION ( 'NONE',  ( -0.1566598588826321192, 0.9876526153536342445, 7.798540720466730171E-17 ) ) ;
#463 = EDGE_CURVE ( 'NONE', #931, #3364, #13273, .T. ) ;
#464 = VECTOR ( 'NONE', #8302, 1000.000000000000000 ) ;
#466 = ORIENTED_EDGE ( 'NONE', *, *, #9742, .F. ) ;
#465 = FACE_OUTER_BOUND ( 'NONE', #17810, .T. ) ;
#467 = EDGE_CURVE ( 'NONE', #9397, #7759, #14260, .T. ) ;
#468 = LINE ( 'NONE', #1619, #12903 ) ;
#469 = EDGE_LOOP ( 'NONE', ( #9333, #3211, #5541, #13498 ) ) ;
#470 = ORIENTED_EDGE ( 'NONE', *, *, #17168, .T. ) ;
#471 = ORIENTED_EDGE ( 'NONE', *, *, #13823, .T. ) ;
#472 = CARTESIAN_POINT ( 'NONE',  ( -38.10636591726526490, -83.99962409888010484, -12.99038105676658539 ) ) ;
#473 = CYLINDRICAL_SURFACE ( 'NONE', #18582, 1.500000000000001554 ) ;
#474 = ORIENTED_EDGE ( 'NONE', *, *, #16472, .T. ) ;
#475 = CYLINDRICAL_SURFACE ( 'NONE', #1700, 1.500000000000000888 ) ;
#476 = CARTESIAN_POINT ( 'NONE',  ( 3.000000000000000000, 4.898587196589412829E-16, -37.00000000000000711 ) ) ;
#477 = AXIS2_PLACEMENT_3D ( 'NONE', #13662, #13565, #10447 ) ;
#478 = DIRECTION ( 'NONE',  ( 0.000000000000000000, 0.000000000000000000, 1.000000000000000000 ) ) ;
#479 = DIRECTION ( 'NONE',  ( -1.000000000000000000, 0.000000000000000000, 0.000000000000000000 ) ) ;
#480 = LINE ( 'NONE', #6273, #9392 ) ;
#481 = CARTESIAN_POINT ( 'NONE',  ( -131.1404785418517918, -2.850701963179328668, -13.78215425775057490 ) ) ;
#482 = VERTEX_POINT ( 'NONE', #1195 ) ;
#483 = FACE_BOUND ( 'NONE', #13486, .T. ) ;
#484 = EDGE_CURVE ( 'NONE', #14364, #13704, #1564, .T. ) ;
#485 = ORIENTED_EDGE ( 'NONE', *, *, #9618, .T. ) ;
#486 = VECTOR ( 'NONE', #9487, 1000.000000000000000 ) ;
#487 = DIRECTION ( 'NONE',  ( -0.9876526153536341335, -0.1566598588826327021, 0.000000000000000000 ) ) ;
#489 = EDGE_CURVE ( 'NONE', #18416, #1139, #6043, .T. ) ;
#488 = DIRECTION ( 'NONE',  ( -0.9876526153536341335, -0.1566598588826327021, 0.000000000000000000 ) ) ;
#490 = CIRCLE ( 'NONE', #15932, 13.78215425775057668 ) ;
#491 = VERTEX_POINT ( 'NONE', #2863 ) ;
#492 = EDGE_CURVE ( 'NONE', #15556, #14764, #2100, .T. ) ;
#493 = EDGE_LOOP ( 'NONE', ( #4032, #9284, #18031, #15546 ) ) ;
#494 = ORIENTED_EDGE ( 'NONE', *, *, #2458, .T. ) ;
#495 = VERTEX_POINT ( 'NONE', #13004 ) ;
#496 = CARTESIAN_POINT ( 'NONE',  ( -174.0670050711101737, 56.28339404658832024, -2.500000000000000000 ) ) ;
#497 = EDGE_LOOP ( 'NONE', ( #2948, #10572, #17851, #2071 ) ) ;
#498 = FACE_BOUND ( 'NONE', #17308, .T. ) ;
#499 = AXIS2_PLACEMENT_3D ( 'NONE', #13270, #3318, #9014 ) ;
#500 = CYLINDRICAL_SURFACE ( 'NONE', #18608, 1.500000000000001554 ) ;
#501 = ORIENTED_EDGE ( 'NONE', *, *, #11049, .F. ) ;
#502 = VECTOR ( 'NONE', #15322, 1000.000000000000000 ) ;
#503 = ORIENTED_EDGE ( 'NONE', *, *, #3380, .F. ) ;
#504 = DIRECTION ( 'NONE',  ( -0.9876526153536341335, -0.1566598588826327021, 0.000000000000000000 ) ) ;
#505 = ORIENTED_EDGE ( 'NONE', *, *, #6048, .T. ) ;
#506 = LINE ( 'NONE', #700, #9084 ) ;
#507 = CARTESIAN_POINT ( 'NONE',  ( -42.38608437559395270, -21.91048909185306925, 8.660254037844417496 ) ) ;
#508 = DIRECTION ( 'NONE',  ( 1.438274729681541867E-16, 6.252920376642369977E-17, -1.000000000000000000 ) ) ;
#509 = DIRECTION ( 'NONE',  ( 0.000000000000000000, 0.000000000000000000, 1.000000000000000000 ) ) ;
#510 = ORIENTED_EDGE ( 'NONE', *, *, #9686, .F. ) ;
#511 = EDGE_LOOP ( 'NONE', ( #3706, #485 ) ) ;
#512 = CARTESIAN_POINT ( 'NONE',  ( 5.481473465377026066, -12.88229205725314586, -19.99999999999999645 ) ) ;
#513 = AXIS2_PLACEMENT_3D ( 'NONE', #14412, #1535, #9778 ) ;
#514 = CARTESIAN_POINT ( 'NONE',  ( -129.1404785418517918, -2.850701963179328668, 9.951701414186818625E-16 ) ) ;
#515 = DIRECTION ( 'NONE',  ( -0.9876526153536336894, -0.1566598588826349503, 0.000000000000000000 ) ) ;
#516 = EDGE_CURVE ( 'NONE', #370, #16376, #2953, .T. ) ;
#517 = DIRECTION ( 'NONE',  ( 0.000000000000000000, 0.000000000000000000, 1.000000000000000000 ) ) ;
#518 = VERTEX_POINT ( 'NONE', #6943 ) ;
#519 = EDGE_CURVE ( 'NONE', #14468, #5881, #4054, .T. ) ;
#520 = VECTOR ( 'NONE', #6791, 1000.000000000000000 ) ;
#521 = ORIENTED_EDGE ( 'NONE', *, *, #3170, .T. ) ;
#522 = DIRECTION ( 'NONE',  ( -0.000000000000000000, -0.000000000000000000, -1.000000000000000000 ) ) ;
#523 = AXIS2_PLACEMENT_3D ( 'NONE', #1578, #2969, #8674 ) ;
#524 = DIRECTION ( 'NONE',  ( -0.1566598588826321747, 0.9876526153536343555, 0.000000000000000000 ) ) ;
#525 = ORIENTED_EDGE ( 'NONE', *, *, #14996, .F. ) ;
#526 = EDGE_CURVE ( 'NONE', #6605, #14798, #15112, .T. ) ;
#527 = CIRCLE ( 'NONE', #10191, 1.500000000000000888 ) ;
#528 = AXIS2_PLACEMENT_3D ( 'NONE', #2893, #8689, #14567 ) ;
#529 = DIRECTION ( 'NONE',  ( -0.1566598588826321192, 0.9876526153536342445, 7.798540720466731404E-17 ) ) ;
#530 = FACE_BOUND ( 'NONE', #4136, .T. ) ;
#531 = EDGE_LOOP ( 'NONE', ( #10532, #13578 ) ) ;
#532 = DIRECTION ( 'NONE',  ( -0.1566598588826321192, 0.9876526153536342445, 7.798540720466731404E-17 ) ) ;
#533 = DIRECTION ( 'NONE',  ( -0.9876526153536341335, -0.1566598588826327021, 0.000000000000000000 ) ) ;
#534 =( GEOMETRIC_REPRESENTATION_CONTEXT ( 3 ) GLOBAL_UNCERTAINTY_ASSIGNED_CONTEXT ( ( #9804 ) ) GLOBAL_UNIT_ASSIGNED_CONTEXT ( ( #13864, #16748, #10928 ) ) REPRESENTATION_CONTEXT ( 'NONE', 'WORKASPACE' ) );
#535 = VECTOR ( 'NONE', #11000, 1000.000000000000000 ) ;
#536 = FACE_OUTER_BOUND ( 'NONE', #6098, .T. ) ;
#537 = VERTEX_POINT ( 'NONE', #4535 ) ;
#538 = DIRECTION ( 'NONE',  ( -0.1566598588826321192, 0.9876526153536342445, 7.798540720466731404E-17 ) ) ;
#539 = ORIENTED_EDGE ( 'NONE', *, *, #13629, .T. ) ;
#540 = AXIS2_PLACEMENT_3D ( 'NONE', #14197, #7021, #18420 ) ;
#541 = ORIENTED_EDGE ( 'NONE', *, *, #18462, .T. ) ;
#542 = ORIENTED_EDGE ( 'NONE', *, *, #10730, .T. ) ;
#543 = EDGE_CURVE ( 'NONE', #4382, #4160, #12054, .T. ) ;
#544 = DIRECTION ( 'NONE',  ( -0.9876526153536344665, -0.1566598588826304539, 0.000000000000000000 ) ) ;
#545 = CARTESIAN_POINT ( 'NONE',  ( -57.20087360589841552, -24.26038697509253694, -8.660254037844380193 ) ) ;
#546 = AXIS2_PLACEMENT_3D ( 'NONE', #4997, #10776, #10699 ) ;
#547 = DIRECTION ( 'NONE',  ( -0.1566598588826321192, 0.9876526153536342445, 7.798540720466730171E-17 ) ) ;
#548 = DIRECTION ( 'NONE',  ( -0.1566598588826321192, 0.9876526153536342445, 7.798540720466731404E-17 ) ) ;
#549 = ORIENTED_EDGE ( 'NONE', *, *, #6994, .F. ) ;
#550 = CARTESIAN_POINT ( 'NONE',  ( -26.74836084069850983, -82.19803572172985184, 21.65063509461101532 ) ) ;
#551 = FILL_AREA_STYLE_COLOUR ( '', #12034 ) ;
#552 = ADVANCED_FACE ( 'NONE', ( #6251 ), #11983, .T. ) ;
#553 = AXIS2_PLACEMENT_3D ( 'NONE', #8026, #3657, #13790 ) ;
#554 = DIRECTION ( 'NONE',  ( -0.1566598588826321192, 0.9876526153536342445, 7.798540720466730171E-17 ) ) ;
#555 = EDGE_CURVE ( 'NONE', #8251, #1903, #12013, .T. ) ;
#556 = CARTESIAN_POINT ( 'NONE',  ( -16.87183468716221313, -80.63143713290354242, 12.99038105676661203 ) ) ;
#557 = AXIS2_PLACEMENT_3D ( 'NONE', #12003, #12293, #13716 ) ;
#558 = LINE ( 'NONE', #16393, #11124 ) ;
#559 = VECTOR ( 'NONE', #18084, 1000.000000000000000 ) ;
#560 = CARTESIAN_POINT ( 'NONE',  ( -43.86756329862440396, -22.14547888017701283, 8.660254037844417496 ) ) ;
#562 = ORIENTED_EDGE ( 'NONE', *, *, #1186, .T. ) ;
#561 = CARTESIAN_POINT ( 'NONE',  ( -42.55080268635658314, -84.70459346385194976, 1.443110928631665584E-14 ) ) ;
#563 = FACE_OUTER_BOUND ( 'NONE', #9796, .T. ) ;
#564 = EDGE_CURVE ( 'NONE', #10544, #13205, #12684, .T. ) ;
#565 = ORIENTED_EDGE ( 'NONE', *, *, #12861, .F. ) ;
#566 = EDGE_LOOP ( 'NONE', ( #4430, #255 ) ) ;
#567 = DIRECTION ( 'NONE',  ( -0.1566598588826321747, 0.9876526153536343555, 0.000000000000000000 ) ) ;
#568 = ADVANCED_FACE ( 'NONE', ( #7048 ), #12876, .F. ) ;
#569 = CIRCLE ( 'NONE', #2365, 150.0000000000000000 ) ;
#570 = CARTESIAN_POINT ( 'NONE',  ( -73.70149508017377116, -31.94019758230671258, -4.330127018922181215 ) ) ;
#571 = VECTOR ( 'NONE', #10120, 1000.000000000000000 ) ;
#572 = EDGE_CURVE ( 'NONE', #12438, #2916, #15328, .T. ) ;
#573 = ORIENTED_EDGE ( 'NONE', *, *, #1192, .T. ) ;
#574 = CARTESIAN_POINT ( 'NONE',  ( -2.200000000000000178, 0.000000000000000000, 25.00000000000000000 ) ) ;
#575 = CIRCLE ( 'NONE', #15701, 2.200000000000000622 ) ;
#576 = ORIENTED_EDGE ( 'NONE', *, *, #17660, .F. ) ;
#577 = CARTESIAN_POINT ( 'NONE',  ( -50.49165861936347000, -28.25869089856487903, 21.65063509461101887 ) ) ;
#578 = CYLINDRICAL_SURFACE ( 'NONE', #1583, 1.500000000000001554 ) ;
#579 = ADVANCED_FACE ( 'NONE', ( #13708 ), #5677, .F. ) ;
#580 = UNCERTAINTY_MEASURE_WITH_UNIT (LENGTH_MEASURE( 1.000000000000000082E-05 ), #14853, 'distance_accuracy_value', 'NONE');
#581 = DIRECTION ( 'NONE',  ( -0.1566598588826321747, 0.9876526153536343555, 0.000000000000000000 ) ) ;
#582 = FACE_OUTER_BOUND ( 'NONE', #8107, .T. ) ;
#583 = CARTESIAN_POINT ( 'NONE',  ( -6.830590222863280658, -16.27073417207831696, 4.330127018922214965 ) ) ;
#584 = VERTEX_POINT ( 'NONE', #8328 ) ;
#585 = CARTESIAN_POINT ( 'NONE',  ( -52.92115514756972061, -86.34952198211959740, -4.330127018922185655 ) ) ;
#586 = ORIENTED_EDGE ( 'NONE', *, *, #12943, .T. ) ;
#587 = FACE_OUTER_BOUND ( 'NONE', #13970, .T. ) ;
#588 = CIRCLE ( 'NONE', #9042, 1.500000000000000888 ) ;
#589 = AXIS2_PLACEMENT_3D ( 'NONE', #10009, #16176, #5934 ) ;
#590 = CARTESIAN_POINT ( 'NONE',  ( -49.79347899074619477, -23.08543803347279422, -21.65063509461098334 ) ) ;
#591 = CIRCLE ( 'NONE', #11158, 1.500000000000001332 ) ;
#592 = VERTEX_POINT ( 'NONE', #4242 ) ;
#593 = ORIENTED_EDGE ( 'NONE', *, *, #12961, .T. ) ;
#594 = ORIENTED_EDGE ( 'NONE', *, *, #8585, .F. ) ;
#595 = CARTESIAN_POINT ( 'NONE',  ( -42.38608437559395270, -21.91048909185306570, 1.926565525561698076E-14 ) ) ;
#596 = EDGE_CURVE ( 'NONE', #7360, #1643, #10020, .T. ) ;
#597 = FACE_BOUND ( 'NONE', #11849, .T. ) ;
#598 = EDGE_CURVE ( 'NONE', #9513, #6519, #16338, .T. ) ;
#599 = AXIS2_PLACEMENT_3D ( 'NONE', #9609, #16835, #3523 ) ;
#600 = ADVANCED_FACE ( 'NONE', ( #10108 ), #4133, .F. ) ;
#601 = EDGE_CURVE ( 'NONE', #8134, #12438, #12857, .T. ) ;
#602 = CARTESIAN_POINT ( 'NONE',  ( -20.86208015875458344, -23.55889513208593655, 4.330127018922217630 ) ) ;
#603 = VECTOR ( 'NONE', #5115, 1000.000000000000000 ) ;
#604 = ORIENTED_EDGE ( 'NONE', *, *, #11122, .T. ) ;
#605 = VECTOR ( 'NONE', #12622, 1000.000000000000000 ) ;
#606 = AXIS2_PLACEMENT_3D ( 'NONE', #12503, #16894, #9679 ) ;
#607 = VECTOR ( 'NONE', #8603, 1000.000000000000000 ) ;
#608 = ORIENTED_EDGE ( 'NONE', *, *, #18557, .T. ) ;
#609 = FACE_BOUND ( 'NONE', #5299, .T. ) ;
#610 = VERTEX_POINT ( 'NONE', #13044 ) ;
#611 = FACE_OUTER_BOUND ( 'NONE', #2046, .T. ) ;
#612 = ORIENTED_EDGE ( 'NONE', *, *, #8796, .F. ) ;
#613 = DIRECTION ( 'NONE',  ( -0.9876526153536336894, -0.1566598588826349503, 0.000000000000000000 ) ) ;
#614 = FACE_OUTER_BOUND ( 'NONE', #5842, .T. ) ;
#615 = AXIS2_PLACEMENT_3D ( 'NONE', #12181, #13417, #453 ) ;
#616 = DIRECTION ( 'NONE',  ( -0.1566598588826321192, 0.9876526153536342445, 7.798540720466730171E-17 ) ) ;
#617 = DIRECTION ( 'NONE',  ( -0.9876526153536336894, -0.1566598588826349503, 0.000000000000000000 ) ) ;
#618 = ORIENTED_EDGE ( 'NONE', *, *, #8953, .T. ) ;
#619 = ORIENTED_EDGE ( 'NONE', *, *, #10277, .T. ) ;
#620 = CARTESIAN_POINT ( 'NONE',  ( -0.5755665338273089349, -78.04654946134009208, -21.65063509461098690 ) ) ;
#621 = AXIS2_PLACEMENT_3D ( 'NONE', #894, #5241, #613 ) ;
#622 = CARTESIAN_POINT ( 'NONE',  ( 0.000000000000000000, 0.000000000000000000, 24.99999999999999289 ) ) ;
#623 = CYLINDRICAL_SURFACE ( 'NONE', #6256, 1.500000000000001554 ) ;
#624 = ORIENTED_EDGE ( 'NONE', *, *, #17746, .T. ) ;
#625 = FACE_OUTER_BOUND ( 'NONE', #8989, .T. ) ;
#626 = VERTEX_POINT ( 'NONE', #5942 ) ;
#627 = VECTOR ( 'NONE', #13045, 1000.000000000000000 ) ;
#628 = FACE_OUTER_BOUND ( 'NONE', #2003, .T. ) ;
#629 = CIRCLE ( 'NONE', #16060, 1.500000000000000888 ) ;
#630 = DIRECTION ( 'NONE',  ( -0.9876526153536341335, -0.1566598588826330907, 0.000000000000000000 ) ) ;
#631 = EDGE_CURVE ( 'NONE', #4650, #2328, #2045, .T. ) ;
#632 = EDGE_LOOP ( 'NONE', ( #12628, #11654, #16155, #8883 ) ) ;
#633 = CIRCLE ( 'NONE', #2130, 1.500000000000000000 ) ;
#634 = ADVANCED_FACE ( 'NONE', ( #824 ), #15404, .T. ) ;
#635 = DIRECTION ( 'NONE',  ( 0.000000000000000000, 0.000000000000000000, 1.000000000000000000 ) ) ;
#636 = VECTOR ( 'NONE', #10205, 1000.000000000000000 ) ;
#637 = CYLINDRICAL_SURFACE ( 'NONE', #5402, 1.500000000000001554 ) ;
#638 = DIRECTION ( 'NONE',  ( 0.000000000000000000, 0.000000000000000000, 1.000000000000000000 ) ) ;
#639 = EDGE_LOOP ( 'NONE', ( #12804, #15222 ) ) ;
#640 = EDGE_LOOP ( 'NONE', ( #4206, #1912, #17476, #10777 ) ) ;
#641 = DIRECTION ( 'NONE',  ( -0.1566598588826321192, 0.9876526153536342445, 7.798540720466730171E-17 ) ) ;
#642 = EDGE_LOOP ( 'NONE', ( #576, #3191 ) ) ;
#643 = AXIS2_PLACEMENT_3D ( 'NONE', #1751, #7726, #1586 ) ;
#644 = CARTESIAN_POINT ( 'NONE',  ( -33.00338452973448966, -20.42222043246806606, 12.99038105676661736 ) ) ;
#645 = ORIENTED_EDGE ( 'NONE', *, *, #717, .T. ) ;
#646 = DIRECTION ( 'NONE',  ( -0.1566598588826321747, 0.9876526153536343555, 0.000000000000000000 ) ) ;
#647 = CARTESIAN_POINT ( 'NONE',  ( 10.28861223506262412, -76.32329101363113466, -8.660254037844389075 ) ) ;
#648 = AXIS2_PLACEMENT_3D ( 'NONE', #10093, #14649, #17614 ) ;
#649 = CYLINDRICAL_SURFACE ( 'NONE', #9079, 1.500000000000001554 ) ;
#650 = CARTESIAN_POINT ( 'NONE',  ( 55.85952145814821534, 6.938893903907228378E-15, -30.00000000000000000 ) ) ;
#651 = DIRECTION ( 'NONE',  ( 0.000000000000000000, 0.000000000000000000, 1.000000000000000000 ) ) ;
#652 = DIRECTION ( 'NONE',  ( -0.1566598588826321747, 0.9876526153536343555, 0.000000000000000000 ) ) ;
#653 = EDGE_CURVE ( 'NONE', #16941, #893, #3016, .T. ) ;
#654 = AXIS2_PLACEMENT_3D ( 'NONE', #15823, #11614, #7302 ) ;
#655 = ADVANCED_FACE ( 'NONE', ( #2425 ), #15585, .F. ) ;
#656 = DIRECTION ( 'NONE',  ( -0.1566598588826321747, 0.9876526153536343555, 0.000000000000000000 ) ) ;
#657 = DIRECTION ( 'NONE',  ( -0.9876526153536336894, -0.1566598588826349503, 0.000000000000000000 ) ) ;
#658 = FACE_BOUND ( 'NONE', #11920, .T. ) ;
#659 = CARTESIAN_POINT ( 'NONE',  ( -84.16561914167408531, -33.59999999999994458, -30.00000000000000000 ) ) ;
#660 = TOROIDAL_SURFACE ( 'NONE', #5229, 12.83663829214476060, 3.000000000000000000 ) ;
#661 = FACE_OUTER_BOUND ( 'NONE', #1913, .T. ) ;
#662 = EDGE_CURVE ( 'NONE', #6476, #14356, #11311, .T. ) ;
#663 = CARTESIAN_POINT ( 'NONE',  ( -33.20773785067495254, -25.51714336811882688, -17.32050807568878170 ) ) ;
#665 = ORIENTED_EDGE ( 'NONE', *, *, #1714, .F. ) ;
#664 = CARTESIAN_POINT ( 'NONE',  ( -49.79347899074619477, -23.08543803347279777, -12.99038105676658006 ) ) ;
#666 = AXIS2_PLACEMENT_3D ( 'NONE', #9517, #14150, #12441 ) ;
#667 = CARTESIAN_POINT ( 'NONE',  ( -64.77298653181324539, -88.22944028871116018, 4.330127018922213189 ) ) ;
#668 = EDGE_LOOP ( 'NONE', ( #10359, #125, #12635, #15355, #1976 ) ) ;
#669 = EDGE_CURVE ( 'NONE', #3382, #9105, #9816, .T. ) ;
#670 = VECTOR ( 'NONE', #1243, 1000.000000000000000 ) ;
#671 = PLANE ( 'NONE',  #9426 ) ;
#672 = ORIENTED_EDGE ( 'NONE', *, *, #2828, .F. ) ;
#673 = CIRCLE ( 'NONE', #17636, 1.500000000000001332 ) ;
#674 = DIRECTION ( 'NONE',  ( -0.9876526153536341335, -0.1566598588826327021, 0.000000000000000000 ) ) ;
#675 = CARTESIAN_POINT ( 'NONE',  ( -70.24471092643608472, -31.39188807621751209, -4.330127018922181215 ) ) ;
#676 = CARTESIAN_POINT ( 'NONE',  ( 0.000000000000000000, 0.000000000000000000, 35.00000000000000000 ) ) ;
#677 = CARTESIAN_POINT ( 'NONE',  ( -21.84973277410820458, -23.71555499096855613, 8.660254037844417496 ) ) ;
#678 = CARTESIAN_POINT ( 'NONE',  ( -129.1404785418517918, -2.850701963179328668, 9.951701414186818625E-16 ) ) ;
#679 = CARTESIAN_POINT ( 'NONE',  ( -70.00000000000000000, 44.99999999999999289, -19.99999999999999645 ) ) ;
#680 = ORIENTED_EDGE ( 'NONE', *, *, #12590, .F. ) ;
#681 =( LENGTH_UNIT ( ) NAMED_UNIT ( * ) SI_UNIT ( .MILLI., .METRE. ) );
#682 = DIRECTION ( 'NONE',  ( -0.5989998693185457634, -0.8007491221077704946, 0.000000000000000000 ) ) ;
#683 = EDGE_CURVE ( 'NONE', #5280, #3602, #11594, .T. ) ;
#684 = DIRECTION ( 'NONE',  ( -0.1566598588826321192, 0.9876526153536342445, 7.798540720466730171E-17 ) ) ;
#685 = CARTESIAN_POINT ( 'NONE',  ( -84.16561914167408531, -33.59999999999994458, 30.00000000000000000 ) ) ;
#686 = AXIS2_PLACEMENT_3D ( 'NONE', #16566, #452, #6525 ) ;
#687 = ORIENTED_EDGE ( 'NONE', *, *, #7447, .F. ) ;
#688 = EDGE_LOOP ( 'NONE', ( #15524, #11717, #9471, #1813 ) ) ;
#689 = EDGE_LOOP ( 'NONE', ( #1640, #7060 ) ) ;
#690 = EDGE_CURVE ( 'NONE', #16087, #855, #10278, .T. ) ;
#691 = ORIENTED_EDGE ( 'NONE', *, *, #6782, .T. ) ;
#692 = EDGE_LOOP ( 'NONE', ( #8385, #4021 ) ) ;
#693 = DIRECTION ( 'NONE',  ( -1.000000000000000000, 0.000000000000000000, 0.000000000000000000 ) ) ;
#694 = FACE_BOUND ( 'NONE', #15508, .T. ) ;
#695 = CYLINDRICAL_SURFACE ( 'NONE', #15624, 1.500000000000001554 ) ;
#696 = DIRECTION ( 'NONE',  ( 0.000000000000000000, 0.000000000000000000, 1.000000000000000000 ) ) ;
#697 = VERTEX_POINT ( 'NONE', #8248 ) ;
#698 = PRESENTATION_LAYER_ASSIGNMENT (  '', '', ( #18286 ) ) ;
#699 = DIRECTION ( 'NONE',  ( -0.1566598588826321192, 0.9876526153536342445, 7.798540720466731404E-17 ) ) ;
#700 = CARTESIAN_POINT ( 'NONE',  ( -28.22983976372896109, -82.43302551005379541, 12.99038105676661203 ) ) ;
#701 = CARTESIAN_POINT ( 'NONE',  ( -79.30363509306917535, 32.43333333333333002, 25.00000000000002132 ) ) ;
#702 = CYLINDRICAL_SURFACE ( 'NONE', #4184, 1.500000000000001554 ) ;
#703 = CARTESIAN_POINT ( 'NONE',  ( 11.59211860341528144, 6.314490184041265053, -130.3485206753969976 ) ) ;
#704 = EDGE_CURVE ( 'NONE', #8986, #862, #12070, .T. ) ;
#705 = EDGE_LOOP ( 'NONE', ( #18497, #13074 ) ) ;
#706 = ORIENTED_EDGE ( 'NONE', *, *, #10496, .T. ) ;
#707 = DIRECTION ( 'NONE',  ( -0.1566598588826321192, 0.9876526153536342445, 7.798540720466731404E-17 ) ) ;
#708 = EDGE_CURVE ( 'NONE', #13151, #10116, #6664, .T. ) ;
#709 = DIRECTION ( 'NONE',  ( -0.1566598588826321192, 0.9876526153536342445, 7.798540720466730171E-17 ) ) ;
#710 = ORIENTED_EDGE ( 'NONE', *, *, #11771, .F. ) ;
#711 = CARTESIAN_POINT ( 'NONE',  ( -48.97054468615517919, -85.72288254658906226, 17.32050807568881368 ) ) ;
#712 = EDGE_CURVE ( 'NONE', #4620, #15439, #5093, .T. ) ;
#713 = CARTESIAN_POINT ( 'NONE',  ( -4.565812005419673802, -20.97400746052251108, 12.99038105676661026 ) ) ;
#714 = ORIENTED_EDGE ( 'NONE', *, *, #10708, .T. ) ;
#715 = DIRECTION ( 'NONE',  ( 0.9868632313631133801, 0.1615579233078775490, 0.000000000000000000 ) ) ;
#716 = DIRECTION ( 'NONE',  ( -2.735665993912342121E-16, -0.000000000000000000, -1.000000000000000000 ) ) ;
#717 = EDGE_CURVE ( 'NONE', #8478, #7247, #7561, .T. ) ;
#718 = CARTESIAN_POINT ( 'NONE',  ( -174.0586467429681363, 56.10169251196822415, -3.278196957010492962 ) ) ;
#719 = VERTEX_POINT ( 'NONE', #12471 ) ;
#720 = FACE_BOUND ( 'NONE', #3866, .T. ) ;
#721 = CARTESIAN_POINT ( 'NONE',  ( -2.096680467035594297, -20.58235781331593017, -8.660254037844383745 ) ) ;
#722 = CARTESIAN_POINT ( 'NONE',  ( -46.50141314777108903, -85.33123289938248490, 21.65063509461101532 ) ) ;
#723 = CARTESIAN_POINT ( 'NONE',  ( -30.73860631229088725, -25.12549372091224598, 21.65063509461101887 ) ) ;
#724 = CYLINDRICAL_SURFACE ( 'NONE', #1811, 1.500000000000001554 ) ;
#725 = CARTESIAN_POINT ( 'NONE',  ( -8.516422466834198346, -21.60064689605303911, -17.32050807568878170 ) ) ;
#726 = CARTESIAN_POINT ( 'NONE',  ( -77.65210554158829837, -32.56683701783724416, -8.660254037844380193 ) ) ;
#727 = EDGE_CURVE ( 'NONE', #16068, #9239, #3604, .T. ) ;
#728 = DIRECTION ( 'NONE',  ( -0.1566598588826321192, 0.9876526153536342445, 7.798540720466731404E-17 ) ) ;
#729 = ADVANCED_FACE ( 'NONE', ( #13640 ), #2185, .F. ) ;
#730 = VERTEX_POINT ( 'NONE', #6878 ) ;
#731 = ORIENTED_EDGE ( 'NONE', *, *, #2510, .T. ) ;
#732 = CARTESIAN_POINT ( 'NONE',  ( 0.000000000000000000, 0.000000000000000000, -35.00000000000000000 ) ) ;
#733 = EDGE_LOOP ( 'NONE', ( #1309, #17633, #9167, #16624 ) ) ;
#734 = CYLINDRICAL_SURFACE ( 'NONE', #16067, 1.500000000000001554 ) ;
#735 = ORIENTED_EDGE ( 'NONE', *, *, #17861, .T. ) ;
#736 = PRODUCT_RELATED_PRODUCT_CATEGORY ( 'part', '', ( #775 ) ) ;
#737 = ORIENTED_EDGE ( 'NONE', *, *, #9685, .F. ) ;
#738 = EDGE_CURVE ( 'NONE', #5480, #5362, #12722, .T. ) ;
#739 = CARTESIAN_POINT ( 'NONE',  ( 3.231158466157545206, -19.73726462726228092, -35.00000000000000000 ) ) ;
#740 = DIRECTION ( 'NONE',  ( -0.9876526153536341335, -0.1566598588826327021, 0.000000000000000000 ) ) ;
#741 = CARTESIAN_POINT ( 'NONE',  ( -72.71384246482016067, -31.78353772342409300, 8.660254037844417496 ) ) ;
#742 = DIRECTION ( 'NONE',  ( 0.000000000000000000, 0.000000000000000000, 1.000000000000000000 ) ) ;
#743 = DIRECTION ( 'NONE',  ( -0.1566598588826321192, 0.9876526153536342445, 7.798540720466731404E-17 ) ) ;
#744 =( LENGTH_UNIT ( ) NAMED_UNIT ( * ) SI_UNIT ( .MILLI., .METRE. ) );
#745 = DIRECTION ( 'NONE',  ( -0.1566598588826321192, 0.9876526153536342445, 7.798540720466730171E-17 ) ) ;
#746 = CARTESIAN_POINT ( 'NONE',  ( -306.0881213225399051, -2.850701963179326448, -15.83618137761393463 ) ) ;
#747 = CARTESIAN_POINT ( 'NONE',  ( -56.91140061916207316, -29.27697998130197732, 21.65063509461101887 ) ) ;
#748 = LINE ( 'NONE', #7752, #16988 ) ;
#750 = ORIENTED_EDGE ( 'NONE', *, *, #11331, .T. ) ;
#749 = DIRECTION ( 'NONE',  ( 0.000000000000000000, 0.000000000000000000, 1.000000000000000000 ) ) ;
#751 = DIRECTION ( 'NONE',  ( 1.000000000000000000, 0.000000000000000000, 0.000000000000000000 ) ) ;
#752 = VECTOR ( 'NONE', #5936, 1000.000000000000000 ) ;
#753 = VERTEX_POINT ( 'NONE', #12822 ) ;
#754 = ADVANCED_FACE ( 'NONE', ( #2793 ), #7079, .F. ) ;
#755 = VERTEX_POINT ( 'NONE', #15859 ) ;
#756 = ORIENTED_EDGE ( 'NONE', *, *, #631, .F. ) ;
#757 = EDGE_CURVE ( 'NONE', #18512, #8290, #1358, .T. ) ;
#758 = CARTESIAN_POINT ( 'NONE',  ( 6.831828081324923474, -76.87160051972034580, 8.660254037844406838 ) ) ;
#759 = ORIENTED_EDGE ( 'NONE', *, *, #8356, .F. ) ;
#760 = DIRECTION ( 'NONE',  ( -0.9876526153536336894, -0.1566598588826349503, 0.000000000000000000 ) ) ;
#761 = ADVANCED_FACE ( 'NONE', ( #14689 ), #17671, .F. ) ;
#762 = DIRECTION ( 'NONE',  ( -0.9876526153536341335, -0.1566598588826327021, 0.000000000000000000 ) ) ;
#763 = ORIENTED_EDGE ( 'NONE', *, *, #17578, .T. ) ;
#764 = FACE_OUTER_BOUND ( 'NONE', #7194, .T. ) ;
#765 = CARTESIAN_POINT ( 'NONE',  ( -128.8626752476364175, -14.87423233749613694, -4.224609204322598011 ) ) ;
#766 = DIRECTION ( 'NONE',  ( -0.000000000000000000, -0.000000000000000000, -1.000000000000000000 ) ) ;
#767 = CIRCLE ( 'NONE', #14675, 1.499999999999999556 ) ;
#768 = CARTESIAN_POINT ( 'NONE',  ( -127.1354840320379225, 9.580137489138413898, -2.662644313562638754 ) ) ;
#769 = DIRECTION ( 'NONE',  ( -0.000000000000000000, -0.000000000000000000, -1.000000000000000000 ) ) ;
#770 = ORIENTED_EDGE ( 'NONE', *, *, #8506, .F. ) ;
#771 = DIRECTION ( 'NONE',  ( 0.000000000000000000, 0.000000000000000000, 1.000000000000000000 ) ) ;
#772 = CARTESIAN_POINT ( 'NONE',  ( -43.86756329862441817, -22.14547888017700217, -17.32050807568878170 ) ) ;
#773 = DIRECTION ( 'NONE',  ( -0.9876526153536341335, -0.1566598588826327021, 0.000000000000000000 ) ) ;
#774 = CARTESIAN_POINT ( 'NONE',  ( -40.08167114797250719, -84.31294381664535820, -4.330127018922185655 ) ) ;
#775 = PRODUCT ( 'BR-825', 'BR-825', '', ( #7281 ) ) ;
#776 = EDGE_LOOP ( 'NONE', ( #9787, #14436, #16293, #12999 ) ) ;
#777 = VERTEX_POINT ( 'NONE', #10233 ) ;
#778 = EDGE_LOOP ( 'NONE', ( #10197, #3952, #17970, #7335 ) ) ;
#779 = EDGE_LOOP ( 'NONE', ( #18617, #8741 ) ) ;
#780 = CARTESIAN_POINT ( 'NONE',  ( 73.09088021254186174, 1.387778780781445676E-14, 25.00000000000000000 ) ) ;
#781 = AXIS2_PLACEMENT_3D ( 'NONE', #9710, #793, #3786 ) ;
#782 = FACE_BOUND ( 'NONE', #531, .T. ) ;
#783 = EDGE_CURVE ( 'NONE', #1828, #11020, #12691, .T. ) ;
#784 = SURFACE_SIDE_STYLE ('',( #16717 ) ) ;
#785 = CIRCLE ( 'NONE', #5003, 1.499999999999999556 ) ;
#786 = CARTESIAN_POINT ( 'NONE',  ( -32.50955822205765600, -20.34389050302674562, -8.660254037844380193 ) ) ;
#787 = EDGE_CURVE ( 'NONE', #17205, #5608, #12280, .T. ) ;
#788 = FACE_BOUND ( 'NONE', #3592, .T. ) ;
#789 = CARTESIAN_POINT ( 'NONE',  ( -131.1055737289773617, -2.850701963179328668, 9.951701414186818625E-16 ) ) ;
#790 = AXIS2_PLACEMENT_3D ( 'NONE', #5797, #17364, #11534 ) ;
#791 = CARTESIAN_POINT ( 'NONE',  ( -70.00000000000000000, 44.99999999999999289, 2.500000000000000000 ) ) ;
#792 = CARTESIAN_POINT ( 'NONE',  ( -29.05277406831996245, -19.79558099693754158, 17.32050807568882078 ) ) ;
#793 = DIRECTION ( 'NONE',  ( -0.1566598588826321747, 0.9876526153536343555, 0.000000000000000000 ) ) ;
#794 = VERTEX_POINT ( 'NONE', #15247 ) ;
#795 = VERTEX_POINT ( 'NONE', #14107 ) ;
#796 = CARTESIAN_POINT ( 'NONE',  ( -40.57549745564934085, -84.39127374608669641, 1.424741226644455312E-14 ) ) ;
#797 = ORIENTED_EDGE ( 'NONE', *, *, #18408, .F. ) ;
#798 = DIRECTION ( 'NONE',  ( -0.1566598588826321192, 0.9876526153536342445, 7.798540720466730171E-17 ) ) ;
#799 = EDGE_LOOP ( 'NONE', ( #13422, #7345, #16257, #5142 ) ) ;
#800 = ORIENTED_EDGE ( 'NONE', *, *, #2006, .T. ) ;
#801 = DIRECTION ( 'NONE',  ( -0.9876526153536336894, -0.1566598588826350336, 0.000000000000000000 ) ) ;
#802 = AXIS2_PLACEMENT_3D ( 'NONE', #11740, #14986, #10707 ) ;
#803 = ORIENTED_EDGE ( 'NONE', *, *, #16114, .T. ) ;
#804 = CARTESIAN_POINT ( 'NONE',  ( -126.1404785418517918, -15.29729532696464922, 2.500000000000000000 ) ) ;
#805 = ORIENTED_EDGE ( 'NONE', *, *, #9038, .T. ) ;
#806 = AXIS2_PLACEMENT_3D ( 'NONE', #11891, #3185, #17730 ) ;
#807 = EDGE_CURVE ( 'NONE', #4830, #12067, #9970, .T. ) ;
#808 = CARTESIAN_POINT ( 'NONE',  ( -9.299721761247353058, -16.66238381928489787, 8.660254037844413944 ) ) ;
#809 = ADVANCED_FACE ( 'NONE', ( #14209 ), #3858, .F. ) ;
#810 = CARTESIAN_POINT ( 'NONE',  ( -48.02252708097940825, -27.86704125135830523, 1.869203119972154228E-14 ) ) ;
#811 = SHAPE_DEFINITION_REPRESENTATION ( #14086, #15677 ) ;
#812 = EDGE_CURVE ( 'NONE', #4040, #5969, #7036, .T. ) ;
#813 = ORIENTED_EDGE ( 'NONE', *, *, #339, .F. ) ;
#814 = CIRCLE ( 'NONE', #2022, 1.499999999999999556 ) ;
#815 = CARTESIAN_POINT ( 'NONE',  ( -22.34355908178503114, -23.79388492040988012, -21.65063509461098334 ) ) ;
#816 = DIRECTION ( 'NONE',  ( 0.000000000000000000, 0.000000000000000000, 1.000000000000000000 ) ) ;
#817 = CARTESIAN_POINT ( 'NONE',  ( -47.98289207080156160, -85.56622268770642847, 12.99038105676661203 ) ) ;
#818 = FACE_OUTER_BOUND ( 'NONE', #1173, .T. ) ;
#819 = ORIENTED_EDGE ( 'NONE', *, *, #8066, .F. ) ;
#820 = ORIENTED_EDGE ( 'NONE', *, *, #55, .F. ) ;
#821 = FACE_OUTER_BOUND ( 'NONE', #16486, .T. ) ;
#822 = COLOUR_RGB ( '', 0.09019608, 0.27058824, 0.51372549) ;
#823 = EDGE_LOOP ( 'NONE', ( #1463, #16116, #18789, #5628 ) ) ;
#824 = FACE_OUTER_BOUND ( 'NONE', #12213, .T. ) ;
#825 = CARTESIAN_POINT ( 'NONE',  ( -40.57549745564932664, -84.39127374608669641, 8.660254037844412167 ) ) ;
#826 = ORIENTED_EDGE ( 'NONE', *, *, #17274, .F. ) ;
#827 = VERTEX_POINT ( 'NONE', #5596 ) ;
#828 = ORIENTED_EDGE ( 'NONE', *, *, #3619, .F. ) ;
#829 = CIRCLE ( 'NONE', #17492, 1.500000000000000000 ) ;
#830 = CIRCLE ( 'NONE', #16252, 2.200000000000007283 ) ;
#831 = CYLINDRICAL_SURFACE ( 'NONE', #12076, 1.500000000000000666 ) ;
#832 = CARTESIAN_POINT ( 'NONE',  ( -51.27495791377664602, -23.32042782179673779, -21.65063509461097979 ) ) ;
#833 = EDGE_CURVE ( 'NONE', #4754, #3060, #17278, .T. ) ;
#834 = ADVANCED_FACE ( 'NONE', ( #14585 ), #14490, .F. ) ;
#835 = DIRECTION ( 'NONE',  ( -0.1566598588826321192, 0.9876526153536342445, 7.798540720466730171E-17 ) ) ;
#836 = CARTESIAN_POINT ( 'NONE',  ( -346.6567719130321166, 10.97801148527007697, 9.951701414186830458E-16 ) ) ;
#837 = AXIS2_PLACEMENT_3D ( 'NONE', #2306, #16934, #3803 ) ;
#838 = ORIENTED_EDGE ( 'NONE', *, *, #18207, .F. ) ;
#839 = DIRECTION ( 'NONE',  ( -0.1566598588826321192, 0.9876526153536342445, 7.798540720466730171E-17 ) ) ;
#840 = AXIS2_PLACEMENT_3D ( 'NONE', #8135, #16786, #5089 ) ;
#841 = DIRECTION ( 'NONE',  ( -0.9876526153536341335, -0.1566598588826327021, 0.000000000000000000 ) ) ;
#842 = FACE_OUTER_BOUND ( 'NONE', #11073, .T. ) ;
#843 = VECTOR ( 'NONE', #10454, 1000.000000000000000 ) ;
#844 = DIRECTION ( 'NONE',  ( -0.000000000000000000, -0.000000000000000000, -1.000000000000000000 ) ) ;
#845 = ORIENTED_EDGE ( 'NONE', *, *, #9764, .T. ) ;
#846 = DIRECTION ( 'NONE',  ( 0.000000000000000000, -1.000000000000000000, 0.000000000000000000 ) ) ;
#847 = CARTESIAN_POINT ( 'NONE',  ( -42.87991068327079347, -21.98881902129437194, -12.99038105676658006 ) ) ;
#849 = EDGE_LOOP ( 'NONE', ( #13453, #13783, #15744, #11573 ) ) ;
#848 = DIRECTION ( 'NONE',  ( -0.1566598588826321192, 0.9876526153536342445, 7.798540720466731404E-17 ) ) ;
#850 = ORIENTED_EDGE ( 'NONE', *, *, #10300, .T. ) ;
#851 = CARTESIAN_POINT ( 'NONE',  ( -5.349111299832828514, -16.03574438375436984, 21.65063509461101177 ) ) ;
#852 = DIRECTION ( 'NONE',  ( -0.9876526153536336894, -0.1566598588826349503, 0.000000000000000000 ) ) ;
#853 = ORIENTED_EDGE ( 'NONE', *, *, #1767, .F. ) ;
#854 = AXIS2_PLACEMENT_3D ( 'NONE', #7811, #428, #17704 ) ;
#855 = VERTEX_POINT ( 'NONE', #13058 ) ;
#856 = DIRECTION ( 'NONE',  ( -0.1566598588826321192, 0.9876526153536342445, 7.798540720466730171E-17 ) ) ;
#857 = EDGE_LOOP ( 'NONE', ( #17739, #13981 ) ) ;
#858 = CARTESIAN_POINT ( 'NONE',  ( -5.349111299832828514, -16.03574438375436984, -12.99038105676658006 ) ) ;
#859 = VERTEX_POINT ( 'NONE', #91 ) ;
#860 = AXIS2_PLACEMENT_3D ( 'NONE', #11980, #10856, #3558 ) ;
#861 = CARTESIAN_POINT ( 'NONE',  ( -129.1404785418517918, -15.35070196317932911, -2.500000000000000000 ) ) ;
#862 = VERTEX_POINT ( 'NONE', #10482 ) ;
#863 = DIRECTION ( 'NONE',  ( 0.000000000000000000, 0.000000000000000000, 1.000000000000000000 ) ) ;
#864 = DIRECTION ( 'NONE',  ( 0.000000000000000000, 0.000000000000000000, 1.000000000000000000 ) ) ;
#865 = VECTOR ( 'NONE', #5049, 1000.000000000000000 ) ;
#866 = DIRECTION ( 'NONE',  ( 1.000000000000000000, -3.469446951953611033E-15, 0.000000000000000000 ) ) ;
#867 = DIRECTION ( 'NONE',  ( -0.1566598588826321192, 0.9876526153536342445, 7.798540720466730171E-17 ) ) ;
#868 = FACE_OUTER_BOUND ( 'NONE', #902, .T. ) ;
#869 = ORIENTED_EDGE ( 'NONE', *, *, #10612, .T. ) ;
#870 = CARTESIAN_POINT ( 'NONE',  ( -77.72973689007648090, 30.96463005215034059, 30.00000000000002842 ) ) ;
#871 = EDGE_LOOP ( 'NONE', ( #12940, #17306, #8437, #16097 ) ) ;
#872 = EDGE_CURVE ( 'NONE', #12166, #14919, #9068, .T. ) ;
#873 = ADVANCED_FACE ( 'NONE', ( #3102 ), #11109, .F. ) ;
#874 = DIRECTION ( 'NONE',  ( -0.9876526153536336894, -0.1566598588826349503, 0.000000000000000000 ) ) ;
#875 = CARTESIAN_POINT ( 'NONE',  ( -48.80582637539256297, -22.92877817459016399, -8.660254037844380193 ) ) ;
#876 = ORIENTED_EDGE ( 'NONE', *, *, #14228, .F. ) ;
#877 = DIRECTION ( 'NONE',  ( -0.9876526153536336894, -0.1566598588826349503, 0.000000000000000000 ) ) ;
#878 = EDGE_CURVE ( 'NONE', #16586, #8364, #5126, .T. ) ;
#879 = ORIENTED_EDGE ( 'NONE', *, *, #394, .F. ) ;
#880 = EDGE_LOOP ( 'NONE', ( #16122, #16267, #14072, #18069 ) ) ;
#881 = ORIENTED_EDGE ( 'NONE', *, *, #6302, .T. ) ;
#882 = DIRECTION ( 'NONE',  ( -0.1566598588826321192, 0.9876526153536342445, 7.798540720466730171E-17 ) ) ;
#883 = VECTOR ( 'NONE', #7257, 1000.000000000000000 ) ;
#884 = FACE_BOUND ( 'NONE', #6398, .T. ) ;
#885 = DIRECTION ( 'NONE',  ( -0.1566598588826321747, 0.9876526153536343555, 0.000000000000000000 ) ) ;
#886 = VERTEX_POINT ( 'NONE', #3551 ) ;
#887 = VECTOR ( 'NONE', #3303, 1000.000000000000000 ) ;
#888 = CYLINDRICAL_SURFACE ( 'NONE', #8455, 1.500000000000001554 ) ;
#889 = AXIS2_PLACEMENT_3D ( 'NONE', #3859, #9849, #13920 ) ;
#890 = EDGE_CURVE ( 'NONE', #98, #3520, #18190, .T. ) ;
#891 = CARTESIAN_POINT ( 'NONE',  ( -34.19539046602857724, -25.67380322700145356, -12.99038105676658006 ) ) ;
#892 = CIRCLE ( 'NONE', #17254, 1.500000000000000888 ) ;
#893 = VERTEX_POINT ( 'NONE', #18016 ) ;
#894 = CARTESIAN_POINT ( 'NONE',  ( -56.37793930130741415, -86.89783148820879433, -12.99038105676658539 ) ) ;
#895 = LINE ( 'NONE', #15645, #17841 ) ;
#896 = CARTESIAN_POINT ( 'NONE',  ( -65.30644784966793281, -30.60858878180435738, -21.65063509461098334 ) ) ;
#897 = VERTEX_POINT ( 'NONE', #15494 ) ;
#898 = VERTEX_POINT ( 'NONE', #6885 ) ;
#899 = DIRECTION ( 'NONE',  ( 0.000000000000000000, 0.000000000000000000, -1.000000000000000000 ) ) ;
#900 = ADVANCED_FACE ( 'NONE', ( #4200 ), #11393, .F. ) ;
#901 = CARTESIAN_POINT ( 'NONE',  ( -168.2745196454702068, 32.00972194781247282, -2.584671478510871090 ) ) ;
#902 = EDGE_LOOP ( 'NONE', ( #12357, #18724, #16202, #3889 ) ) ;
#903 = VECTOR ( 'NONE', #7351, 1000.000000000000000 ) ;
#904 = ORIENTED_EDGE ( 'NONE', *, *, #17050, .F. ) ;
#905 = CARTESIAN_POINT ( 'NONE',  ( -55.42992169613163611, -29.04199019297804085, -4.330127018922181215 ) ) ;
#906 = AXIS2_PLACEMENT_3D ( 'NONE', #274, #1790, #11900 ) ;
#907 = ORIENTED_EDGE ( 'NONE', *, *, #8935, .T. ) ;
#908 = CARTESIAN_POINT ( 'NONE',  ( -2.590506774712417748, -20.66068774275724707, 21.65063509461101177 ) ) ;
#909 = EDGE_CURVE ( 'NONE', #15855, #10665, #14442, .T. ) ;
#910 = ORIENTED_EDGE ( 'NONE', *, *, #2829, .F. ) ;
#911 = CIRCLE ( 'NONE', #16330, 1.500000000000001332 ) ;
#912 = VECTOR ( 'NONE', #7964, 1000.000000000000000 ) ;
#913 = DIRECTION ( 'NONE',  ( -0.1566598588826321747, 0.9876526153536343555, 0.000000000000000000 ) ) ;
#914 = DIRECTION ( 'NONE',  ( -0.1566598588826321192, 0.9876526153536342445, 7.798540720466730171E-17 ) ) ;
#915 = LINE ( 'NONE', #14158, #348 ) ;
#916 = AXIS2_PLACEMENT_3D ( 'NONE', #13711, #15331, #3949 ) ;
#917 = DIRECTION ( 'NONE',  ( -0.1566598588826321192, 0.9876526153536342445, 7.798540720466730171E-17 ) ) ;
#919 = FACE_OUTER_BOUND ( 'NONE', #18493, .T. ) ;
#918 = CIRCLE ( 'NONE', #5451, 150.0000000000000284 ) ;
#920 = DIRECTION ( 'NONE',  ( 0.000000000000000000, 0.000000000000000000, 1.000000000000000000 ) ) ;
#921 = LINE ( 'NONE', #18672, #18060 ) ;
#922 = CARTESIAN_POINT ( 'NONE',  ( -129.1404785418517918, -2.850701963179328668, 9.951701414186818625E-16 ) ) ;
#923 = ORIENTED_EDGE ( 'NONE', *, *, #11613, .T. ) ;
#924 = ORIENTED_EDGE ( 'NONE', *, *, #12167, .F. ) ;
#925 = DIRECTION ( 'NONE',  ( -0.1566598588826321747, 0.9876526153536343555, 0.000000000000000000 ) ) ;
#926 = DIRECTION ( 'NONE',  ( -0.1566598588826321747, 0.9876526153536343555, 0.000000000000000000 ) ) ;
#927 = ADVANCED_FACE ( 'NONE', ( #17116 ), #14530, .T. ) ;
#928 = CIRCLE ( 'NONE', #9702, 1.500000000000001332 ) ;
#929 = ORIENTED_EDGE ( 'NONE', *, *, #10244, .F. ) ;
#930 = ORIENTED_EDGE ( 'NONE', *, *, #11892, .T. ) ;
#931 = VERTEX_POINT ( 'NONE', #7355 ) ;
#932 = DIRECTION ( 'NONE',  ( -0.9876526153536341335, -0.1566598588826327021, 0.000000000000000000 ) ) ;
#933 = ADVANCED_FACE ( 'NONE', ( #17778, #2013, #3142, #13463, #416, #7623, #6298, #17491, #8934, #4756, #7798, #4478, #609, #16055, #12129, #17969, #3700, #6484, #2200, #16910, #12222, #5020, #10800, #16616, #788, #9500, #15268, #2284, #14238, #6958, #1361, #14418, #11557, #11368, #12807, #18648, #5617, #2772, #7235, #7141, #17384, #12889, #7600, #13257, #483, #17466, #4454, #291, #9106, #11832, #17758, #16030, #3041, #1634, #5980, #4556, #10778, #6376, #6552, #13535, #3488, #9386, #10976, #1991, #7874, #3681, #11067, #7776, #3767, #2267, #11535, #15453, #18631, #8543, #1343, #11164, #1430, #5599, #10035, #18535, #4051, #9853, #4258, #7125, #8897, #13146, #6160, #4709, #1521, #1691, #10486, #458, #4530, #6248, #17365, #17447, #16005, #3015, #658, #18019, #9356, #2161, #12273, #18112, #16392, #10854, #3656, #8025, #11978, #17824, #10367, #14557, #5930, #338, #17509, #236, #17794, #16169, #1750, #7641, #4773, #16358, #9151, #5159, #18186, #720, #15012, #16838, #3800, #9611, #2219, #12238, #2030, #5045, #10817, #15385, #2403, #8943, #1389, #17226, #1574, #4586, #13196, #12916, #6011, #16158, #13294, #15787, #13017, #1282, #2854, #120, #14424, #13171, #1452, #7066, #5623, #5824, #11564, #17390, #4375, #15935, #14526, #1551, #11118, #17127, #4103, #10936, #16943, #5557, #3914, #4011, #5459, #2518, #18299, #11219, #6997, #18390, #2317, #8305, #15301, #8388 ), #13873, .F. ) ;
#934 = AXIS2_PLACEMENT_3D ( 'NONE', #18591, #925, #11307 ) ;
#935 = VECTOR ( 'NONE', #846, 1000.000000000000000 ) ;
#936 = CARTESIAN_POINT ( 'NONE',  ( 5.350349158294472218, -77.10659030804430358, 8.660254037844406838 ) ) ;
#937 = CIRCLE ( 'NONE', #15133, 1.500000000000001332 ) ;
#938 = DIRECTION ( 'NONE',  ( -0.9876526153536336894, -0.1566598588826349503, 0.000000000000000000 ) ) ;
#939 = LINE ( 'NONE', #10844, #13609 ) ;
#940 = CARTESIAN_POINT ( 'NONE',  ( -41.39843176024032800, -21.75382923297042836, -4.330127018922180326 ) ) ;
#941 = AXIS2_PLACEMENT_3D ( 'NONE', #8136, #17532, #7463 ) ;
#942 = CARTESIAN_POINT ( 'NONE',  ( -24.27922930231443743, -81.80638607452326028, -17.32050807568878525 ) ) ;
#943 = FILL_AREA_STYLE ('',( #2157 ) ) ;
#944 = CYLINDRICAL_SURFACE ( 'NONE', #1796, 1.500000000000001554 ) ;
#945 = EDGE_CURVE ( 'NONE', #17224, #18075, #18675, .T. ) ;
#946 = CARTESIAN_POINT ( 'NONE',  ( -44.85521591397802155, -22.30213873905964661, 4.330127018922218518 ) ) ;
#947 = AXIS2_PLACEMENT_3D ( 'NONE', #13306, #1941, #340 ) ;
#948 = DIRECTION ( 'NONE',  ( 0.000000000000000000, 0.000000000000000000, 1.000000000000000000 ) ) ;
#949 = VERTEX_POINT ( 'NONE', #14168 ) ;
#950 = DIRECTION ( 'NONE',  ( -0.1566598588826321192, 0.9876526153536342445, 7.798540720466730171E-17 ) ) ;
#951 = CIRCLE ( 'NONE', #3049, 1.500000000000000888 ) ;
#952 = EDGE_CURVE ( 'NONE', #7902, #17807, #2411, .T. ) ;
#953 = ORIENTED_EDGE ( 'NONE', *, *, #7118, .F. ) ;
#954 = ORIENTED_EDGE ( 'NONE', *, *, #1714, .T. ) ;
#955 = EDGE_CURVE ( 'NONE', #4610, #5412, #8486, .T. ) ;
#956 = DIRECTION ( 'NONE',  ( -0.1566598588826321747, 0.9876526153536343555, 0.000000000000000000 ) ) ;
#957 = EDGE_CURVE ( 'NONE', #12710, #4380, #15759, .T. ) ;
#958 = FACE_OUTER_BOUND ( 'NONE', #9602, .T. ) ;
#959 = VERTEX_POINT ( 'NONE', #1210 ) ;
#960 = EDGE_CURVE ( 'NONE', #15970, #4650, #1538, .T. ) ;
#961 = AXIS2_PLACEMENT_3D ( 'NONE', #18768, #147, #1663 ) ;
#962 = EDGE_LOOP ( 'NONE', ( #982, #2651 ) ) ;
#963 = DIRECTION ( 'NONE',  ( 0.000000000000000000, 0.000000000000000000, 1.000000000000000000 ) ) ;
#964 = ORIENTED_EDGE ( 'NONE', *, *, #1067, .F. ) ;
#965 = CIRCLE ( 'NONE', #654, 1.500000000000000888 ) ;
#966 = CARTESIAN_POINT ( 'NONE',  ( -47.03487446562579777, -27.71038139247566789, -21.65063509461098334 ) ) ;
#967 = CIRCLE ( 'NONE', #3346, 2.000000000000001776 ) ;
#968 = VERTEX_POINT ( 'NONE', #6707 ) ;
#969 = DIRECTION ( 'NONE',  ( -0.1566598588826321192, 0.9876526153536342445, 7.798540720466730171E-17 ) ) ;
#970 = CYLINDRICAL_SURFACE ( 'NONE', #18454, 42.89102435249441925 ) ;
#971 = CARTESIAN_POINT ( 'NONE',  ( -9.464440072009985272, -79.45648819128378193, 8.660254037844412167 ) ) ;
#972 = CARTESIAN_POINT ( 'NONE',  ( -68.72359699322777260, -88.85607972424168111, -17.32050807568878525 ) ) ;
#973 = CARTESIAN_POINT ( 'NONE',  ( -7.982961148979534016, -79.22149840295983836, 1.443110928631665584E-14 ) ) ;
#974 = AXIS2_PLACEMENT_3D ( 'NONE', #15485, #9425, #17025 ) ;
#975 =( NAMED_UNIT ( * ) SI_UNIT ( $, .STERADIAN. ) SOLID_ANGLE_UNIT ( ) );
#976 = DIRECTION ( 'NONE',  ( -0.1566598588826321747, 0.9876526153536343555, 0.000000000000000000 ) ) ;
#977 = CIRCLE ( 'NONE', #11525, 3.000000000000004441 ) ;
#978 = EDGE_CURVE ( 'NONE', #14250, #3442, #3727, .T. ) ;
#979 = AXIS2_PLACEMENT_3D ( 'NONE', #8665, #13009, #11657 ) ;
#980 = EDGE_CURVE ( 'NONE', #15050, #12253, #16678, .T. ) ;
#981 = DIRECTION ( 'NONE',  ( -0.1566598588826321192, 0.9876526153536342445, 7.798540720466731404E-17 ) ) ;
#982 = ORIENTED_EDGE ( 'NONE', *, *, #17143, .F. ) ;
#983 = VERTEX_POINT ( 'NONE', #1306 ) ;
#984 = ORIENTED_EDGE ( 'NONE', *, *, #17637, .F. ) ;
#985 = EDGE_LOOP ( 'NONE', ( #11976, #13924 ) ) ;
#986 = CARTESIAN_POINT ( 'NONE',  ( -129.1404785418517918, -2.850701963179328668, 9.951701414186818625E-16 ) ) ;
#987 = VECTOR ( 'NONE', #3572, 1000.000000000000000 ) ;
#988 = EDGE_LOOP ( 'NONE', ( #7419, #3433, #3820, #3749 ) ) ;
#989 = FACE_BOUND ( 'NONE', #4224, .T. ) ;
#990 = EDGE_CURVE ( 'NONE', #13999, #9162, #7089, .T. ) ;
#991 = LINE ( 'NONE', #6761, #9455 ) ;
#992 = ORIENTED_EDGE ( 'NONE', *, *, #3502, .T. ) ;
#993 = CIRCLE ( 'NONE', #7939, 1.500000000000000444 ) ;
#994 = DIRECTION ( 'NONE',  ( -0.1566598588826321747, 0.9876526153536343555, 0.000000000000000000 ) ) ;
#995 = CARTESIAN_POINT ( 'NONE',  ( -78.43540483600145308, -27.62857394106912068, 8.660254037844417496 ) ) ;
#996 = AXIS2_PLACEMENT_3D ( 'NONE', #6812, #18219, #10951 ) ;
#997 = CARTESIAN_POINT ( 'NONE',  ( 73.09088021254186174, 1.387778780781445676E-14, 7.500000000000000000 ) ) ;
#998 = CARTESIAN_POINT ( 'NONE',  ( 73.09088021254186174, 1.387778780781445676E-14, -7.500000000000000000 ) ) ;
#999 = VERTEX_POINT ( 'NONE', #11022 ) ;
#1000 = LINE ( 'NONE', #6771, #7871 ) ;
#1001 = CARTESIAN_POINT ( 'NONE',  ( -33.16810284049710589, -83.21632480446696434, 12.99038105676661203 ) ) ;
#1002 = DIRECTION ( 'NONE',  ( -0.9876526153536341335, -0.1566598588826327021, 0.000000000000000000 ) ) ;
#1003 = EDGE_LOOP ( 'NONE', ( #17375, #14071 ) ) ;
#1004 = CARTESIAN_POINT ( 'NONE',  ( -6.995308533625909320, -79.06483854407721878, -4.330127018922185655 ) ) ;
#1005 = CARTESIAN_POINT ( 'NONE',  ( -53.74408945216072198, -23.71207746900332225, -8.660254037844380193 ) ) ;
#1006 = AXIS2_PLACEMENT_3D ( 'NONE', #3862, #6839, #17082 ) ;
#1007 = ORIENTED_EDGE ( 'NONE', *, *, #957, .F. ) ;
#1008 = ORIENTED_EDGE ( 'NONE', *, *, #2884, .T. ) ;
#1009 = CARTESIAN_POINT ( 'NONE',  ( -41.56315007100295844, -84.54793360496931598, 4.330127018922213189 ) ) ;
#1010 = ORIENTED_EDGE ( 'NONE', *, *, #8263, .T. ) ;
#1011 = LINE ( 'NONE', #12528, #2152 ) ;
#1012 = ADVANCED_FACE ( 'NONE', ( #3813 ), #9628, .F. ) ;
#1013 = EDGE_LOOP ( 'NONE', ( #16793, #1076 ) ) ;
#1014 = CIRCLE ( 'NONE', #11559, 1.500000000000000444 ) ;
#1015 = ADVANCED_FACE ( 'NONE', ( #2544 ), #14301, .T. ) ;
#1016 = VECTOR ( 'NONE', #13635, 1000.000000000000000 ) ;
#1017 = DIRECTION ( 'NONE',  ( -0.1566598588826321192, 0.9876526153536342445, 7.798540720466730171E-17 ) ) ;
#1018 = EDGE_CURVE ( 'NONE', #16065, #3908, #5469, .T. ) ;
#1019 = CARTESIAN_POINT ( 'NONE',  ( 0.4120860815263194254, -77.88988960245745830, 1.077796531449093893E-14 ) ) ;
#1020 = DIRECTION ( 'NONE',  ( -0.000000000000000000, -0.000000000000000000, -1.000000000000000000 ) ) ;
#1021 = DIRECTION ( 'NONE',  ( 0.8752966661511993873, -0.4835863379217779645, 2.050648130084447850E-16 ) ) ;
#1022 = ORIENTED_EDGE ( 'NONE', *, *, #8831, .T. ) ;
#1023 = FACE_OUTER_BOUND ( 'NONE', #12507, .T. ) ;
#1024 = DIRECTION ( 'NONE',  ( 0.000000000000000000, 0.000000000000000000, 1.000000000000000000 ) ) ;
#1025 = CYLINDRICAL_SURFACE ( 'NONE', #1765, 150.0000000000000000 ) ;
#1026 = CARTESIAN_POINT ( 'NONE',  ( 0.000000000000000000, 0.000000000000000000, 35.00000000000000000 ) ) ;
#1027 = EDGE_LOOP ( 'NONE', ( #5119, #9867, #15090, #4924 ) ) ;
#1028 = VERTEX_POINT ( 'NONE', #18426 ) ;
#1029 = VECTOR ( 'NONE', #16300, 1000.000000000000000 ) ;
#1030 = CARTESIAN_POINT ( 'NONE',  ( -84.16561914167408531, -33.59999999999994458, 30.00000000000000000 ) ) ;
#1031 = LINE ( 'NONE', #12349, #14856 ) ;
#1032 = ORIENTED_EDGE ( 'NONE', *, *, #5749, .T. ) ;
#1033 = ORIENTED_EDGE ( 'NONE', *, *, #17505, .T. ) ;
#1034 = CARTESIAN_POINT ( 'NONE',  ( -66.25446545484369665, -88.46443007703511796, 4.330127018922213189 ) ) ;
#1035 = LINE ( 'NONE', #12355, #2442 ) ;
#1036 = EDGE_LOOP ( 'NONE', ( #5576, #5988 ) ) ;
#1037 = ORIENTED_EDGE ( 'NONE', *, *, #6093, .T. ) ;
#1038 = ORIENTED_EDGE ( 'NONE', *, *, #11314, .T. ) ;
#1039 = LINE ( 'NONE', #5277, #7907 ) ;
#1040 = CYLINDRICAL_SURFACE ( 'NONE', #3177, 1.500000000000001554 ) ;
#1041 = CARTESIAN_POINT ( 'NONE',  ( -7.034943543803747090, -21.36565710772908488, 1.540628126764003082E-14 ) ) ;
#1042 = DIRECTION ( 'NONE',  ( -0.9876526153536341335, -0.1566598588826327021, 0.000000000000000000 ) ) ;
#1043 = AXIS2_PLACEMENT_3D ( 'NONE', #16101, #1684, #10478 ) ;
#1044 = DIRECTION ( 'NONE',  ( -0.9876526153536341335, -0.1566598588826327021, 0.000000000000000000 ) ) ;
#1045 = EDGE_CURVE ( 'NONE', #7610, #7134, #15447, .T. ) ;
#1046 = CARTESIAN_POINT ( 'NONE',  ( -61.35583738825340561, -29.98194934627382224, 8.660254037844417496 ) ) ;
#1047 = CARTESIAN_POINT ( 'NONE',  ( -76.17062661855784711, -32.33184722951329348, -8.660254037844380193 ) ) ;
#1048 = DIRECTION ( 'NONE',  ( -8.693966348389027220E-17, 1.991237296706375196E-16, -1.000000000000000000 ) ) ;
#1049 = ORIENTED_EDGE ( 'NONE', *, *, #16408, .F. ) ;
#1050 = CARTESIAN_POINT ( 'NONE',  ( -5.059638313096497697, -21.05233738996382797, 17.32050807568881012 ) ) ;
#1051 = ADVANCED_FACE ( 'NONE', ( #958 ), #2344, .F. ) ;
#1052 = DIRECTION ( 'NONE',  ( -0.9876526153536341335, -0.1566598588826327021, 0.000000000000000000 ) ) ;
#1053 = ORIENTED_EDGE ( 'NONE', *, *, #2494, .F. ) ;
#1054 = DIRECTION ( 'NONE',  ( 0.000000000000000000, 0.000000000000000000, 1.000000000000000000 ) ) ;
#1055 = CARTESIAN_POINT ( 'NONE',  ( -70.24471092643608472, -31.39188807621751209, -12.99038105676658006 ) ) ;
#1057 = ORIENTED_EDGE ( 'NONE', *, *, #8341, .F. ) ;
#1056 = FACE_OUTER_BOUND ( 'NONE', #254, .T. ) ;
#1058 = CARTESIAN_POINT ( 'NONE',  ( 2.200000000000000178, 2.694222958124177006E-16, 25.00000000000000000 ) ) ;
#1059 = DIRECTION ( 'NONE',  ( -0.9876526153536336894, -0.1566598588826349503, 0.000000000000000000 ) ) ;
#1060 = ORIENTED_EDGE ( 'NONE', *, *, #5810, .T. ) ;
#1061 = ORIENTED_EDGE ( 'NONE', *, *, #6669, .F. ) ;
#1062 = DIRECTION ( 'NONE',  ( -0.1566598588826321747, 0.9876526153536343555, 0.000000000000000000 ) ) ;
#1063 = VERTEX_POINT ( 'NONE', #4134 ) ;
#1064 = CARTESIAN_POINT ( 'NONE',  ( -167.4745151998187680, 32.15905408292213252, 2.500000000000000000 ) ) ;
#1065 = DIRECTION ( 'NONE',  ( -0.1566598588826321192, 0.9876526153536342445, 7.798540720466730171E-17 ) ) ;
#1066 = CARTESIAN_POINT ( 'NONE',  ( -37.61253960958842413, -83.92129416943879505, 17.32050807568881368 ) ) ;
#1067 = EDGE_CURVE ( 'NONE', #2946, #18001, #15606, .T. ) ;
#1068 = EDGE_CURVE ( 'NONE', #5828, #8019, #7573, .T. ) ;
#1069 = DIRECTION ( 'NONE',  ( 0.000000000000000000, 0.000000000000000000, 1.000000000000000000 ) ) ;
#1070 = CARTESIAN_POINT ( 'NONE',  ( -79.50968810220766159, 31.87664632526870889, -35.00000000000000000 ) ) ;
#1071 = ADVANCED_FACE ( 'NONE', ( #5585 ), #1143, .F. ) ;
#1072 = FACE_OUTER_BOUND ( 'NONE', #248, .T. ) ;
#1073 = ORIENTED_EDGE ( 'NONE', *, *, #10640, .T. ) ;
#1074 = DIRECTION ( 'NONE',  ( 0.000000000000000000, 0.000000000000000000, 1.000000000000000000 ) ) ;
#1075 = ORIENTED_EDGE ( 'NONE', *, *, #5040, .F. ) ;
#1076 = ORIENTED_EDGE ( 'NONE', *, *, #2727, .T. ) ;
#1077 = ORIENTED_EDGE ( 'NONE', *, *, #15950, .T. ) ;
#1078 = CARTESIAN_POINT ( 'NONE',  ( -36.62488699423481364, -83.76463431055616127, -4.330127018922185655 ) ) ;
#1079 = FACE_BOUND ( 'NONE', #10545, .T. ) ;
#1080 = EDGE_CURVE ( 'NONE', #14612, #18673, #6076, .T. ) ;
#1081 = DIRECTION ( 'NONE',  ( -0.9876526153536341335, -0.1566598588826327021, 0.000000000000000000 ) ) ;
#1082 = VECTOR ( 'NONE', #17061, 1000.000000000000000 ) ;
#1083 = EDGE_CURVE ( 'NONE', #12177, #4657, #17900, .T. ) ;
#1084 = CARTESIAN_POINT ( 'NONE',  ( -170.4124675745486570, 31.54971992778986234, -5.500000000000000000 ) ) ;
#1085 = EDGE_LOOP ( 'NONE', ( #9067, #11367 ) ) ;
#1086 = ADVANCED_FACE ( 'NONE', ( #11427 ), #1507, .F. ) ;
#1087 = DIRECTION ( 'NONE',  ( -0.1566598588826321747, 0.9876526153536343555, 0.000000000000000000 ) ) ;
#1088 = CARTESIAN_POINT ( 'NONE',  ( -72.01566283620284992, -26.61028485833201884, 8.660254037844417496 ) ) ;
#1089 = DIRECTION ( 'NONE',  ( -0.1566598588826321192, 0.9876526153536342445, 7.798540720466731404E-17 ) ) ;
#1090 = ORIENTED_EDGE ( 'NONE', *, *, #6326, .F. ) ;
#1091 = CARTESIAN_POINT ( 'NONE',  ( -51.47931123471711601, -28.41535075744751282, -8.660254037844380193 ) ) ;
#1092 = AXIS2_PLACEMENT_3D ( 'NONE', #1303, #15296, #15670 ) ;
#1093 = CARTESIAN_POINT ( 'NONE',  ( -71.02801022084922522, -26.45362499944937085, -21.65063509461097979 ) ) ;
#1094 = ORIENTED_EDGE ( 'NONE', *, *, #9224, .T. ) ;
#1095 = VERTEX_POINT ( 'NONE', #11610 ) ;
#1096 = DIRECTION ( 'NONE',  ( -0.1566598588826321192, 0.9876526153536342445, 7.798540720466730171E-17 ) ) ;
#1097 = EDGE_LOOP ( 'NONE', ( #10806, #13544, #9035, #12463 ) ) ;
#1098 = LINE ( 'NONE', #18475, #1570 ) ;
#1099 = CARTESIAN_POINT ( 'NONE',  ( -170.5500158571522320, 32.36820283781686669, 5.132104245558541500 ) ) ;
#1100 = ORIENTED_EDGE ( 'NONE', *, *, #16560, .T. ) ;
#1101 = CIRCLE ( 'NONE', #10147, 1.500000000000000888 ) ;
#1102 = DIRECTION ( 'NONE',  ( -0.9876526153536341335, -0.1566598588826327021, 0.000000000000000000 ) ) ;
#1103 = CARTESIAN_POINT ( 'NONE',  ( -70.00000000000000000, 44.99999999999999289, 7.500000000000007105 ) ) ;
#1104 = PRESENTATION_STYLE_ASSIGNMENT (( #9432 ) ) ;
#1105 = CARTESIAN_POINT ( 'NONE',  ( -54.44226908077799720, -28.88533033409540351, 17.32050807568881723 ) ) ;
#1106 = CARTESIAN_POINT ( 'NONE',  ( -45.01993422474066620, -85.09624311105852712, -4.330127018922185655 ) ) ;
#1107 = ORIENTED_EDGE ( 'NONE', *, *, #6048, .F. ) ;
#1108 = EDGE_CURVE ( 'NONE', #2286, #13042, #7003, .T. ) ;
#1109 = DIRECTION ( 'NONE',  ( -0.1566598588826321192, 0.9876526153536342445, 7.798540720466730171E-17 ) ) ;
#1110 = DIRECTION ( 'NONE',  ( 0.000000000000000000, 0.000000000000000000, 1.000000000000000000 ) ) ;
#1111 = EDGE_LOOP ( 'NONE', ( #10380, #9692, #2653, #16288 ) ) ;
#1112 = ADVANCED_FACE ( 'NONE', ( #15817 ), #17434, .F. ) ;
#1113 = VERTEX_POINT ( 'NONE', #14393 ) ;
#1114 = DIRECTION ( 'NONE',  ( -0.9876526153536342445, -0.1566598588826321470, 0.000000000000000000 ) ) ;
#1115 = CARTESIAN_POINT ( 'NONE',  ( -59.83472345504510770, -87.44614099429799126, -12.99038105676658539 ) ) ;
#1116 = VECTOR ( 'NONE', #4946, 1000.000000000000000 ) ;
#1117 = ORIENTED_EDGE ( 'NONE', *, *, #3693, .T. ) ;
#1118 = ORIENTED_EDGE ( 'NONE', *, *, #3119, .T. ) ;
#1119 = EDGE_CURVE ( 'NONE', #5250, #17961, #1414, .T. ) ;
#1120 = ORIENTED_EDGE ( 'NONE', *, *, #2436, .T. ) ;
#1121 = CIRCLE ( 'NONE', #15923, 150.0000000000000000 ) ;
#1122 = ORIENTED_EDGE ( 'NONE', *, *, #6807, .F. ) ;
#1123 = CARTESIAN_POINT ( 'NONE',  ( -57.85941822433786541, -87.13282127653273790, -12.99038105676658539 ) ) ;
#1124 = DIRECTION ( 'NONE',  ( -1.000000000000000000, 0.000000000000000000, 0.000000000000000000 ) ) ;
#1125 = ORIENTED_EDGE ( 'NONE', *, *, #15181, .T. ) ;
#1126 = CARTESIAN_POINT ( 'NONE',  ( -11.76885329963143079, -17.05403346649147878, 4.330127018922214965 ) ) ;
#1127 = AXIS2_PLACEMENT_3D ( 'NONE', #16323, #3218, #17682 ) ;
#1128 = CARTESIAN_POINT ( 'NONE',  ( 0.000000000000000000, 0.000000000000000000, 25.00000000000000000 ) ) ;
#1129 = FACE_OUTER_BOUND ( 'NONE', #12163, .T. ) ;
#1130 = CARTESIAN_POINT ( 'NONE',  ( -65.23030399291528170, -43.49999999999991473, 19.99999999999993605 ) ) ;
#1131 = CARTESIAN_POINT ( 'NONE',  ( 5.350349158294472218, -77.10659030804430358, -8.660254037844389075 ) ) ;
#1132 = VERTEX_POINT ( 'NONE', #18787 ) ;
#1133 = DIRECTION ( 'NONE',  ( -0.1566598588826321192, 0.9876526153536342445, 7.798540720466731404E-17 ) ) ;
#1134 = CARTESIAN_POINT ( 'NONE',  ( -43.08426400421124924, -27.08374195694514341, 8.660254037844417496 ) ) ;
#1135 = EDGE_LOOP ( 'NONE', ( #3407, #12333, #11137, #11919 ) ) ;
#1136 = ORIENTED_EDGE ( 'NONE', *, *, #4437, .T. ) ;
#1137 = CARTESIAN_POINT ( 'NONE',  ( -80.37374032648909861, 30.90317544272717498, 35.00001199999999102 ) ) ;
#1138 = DIRECTION ( 'NONE',  ( -0.1566598588826321192, 0.9876526153536342445, 7.798540720466730171E-17 ) ) ;
#1139 = VERTEX_POINT ( 'NONE', #2826 ) ;
#1140 = CIRCLE ( 'NONE', #2930, 1.500000000000000888 ) ;
#1141 = CIRCLE ( 'NONE', #7183, 1.500000000000001332 ) ;
#1142 = ADVANCED_FACE ( 'NONE', ( #1602 ), #8884, .F. ) ;
#1143 = CYLINDRICAL_SURFACE ( 'NONE', #11190, 145.0000000000000284 ) ;
#1144 = ORIENTED_EDGE ( 'NONE', *, *, #12791, .F. ) ;
#1145 = CIRCLE ( 'NONE', #17485, 1.499999999999999556 ) ;
#1146 = CARTESIAN_POINT ( 'NONE',  ( -33.20773785067495965, -25.51714336811882688, 8.660254037844417496 ) ) ;
#1147 = EDGE_CURVE ( 'NONE', #13568, #2699, #5943, .T. ) ;
#1148 = CIRCLE ( 'NONE', #7487, 1.500000000000001332 ) ;
#1149 = ORIENTED_EDGE ( 'NONE', *, *, #1553, .F. ) ;
#1150 = B_SPLINE_CURVE_WITH_KNOTS ( 'NONE', 3,
 ( #99, #8902, #14865, #6255 ),
 .UNSPECIFIED., .F., .F.,
 ( 4, 4 ),
 ( 0.000000000000000000, 0.003000475340473869428 ),
 .UNSPECIFIED. ) ;
#1151 = DIRECTION ( 'NONE',  ( -0.9826218788918642533, -0.1856185419698762884, 0.000000000000000000 ) ) ;
#1152 = DIRECTION ( 'NONE',  ( -0.000000000000000000, -0.000000000000000000, -1.000000000000000000 ) ) ;
#1153 = CARTESIAN_POINT ( 'NONE',  ( -128.4401431403265121, 9.376841461187488846, -3.563338245596201048 ) ) ;
#1154 = ORIENTED_EDGE ( 'NONE', *, *, #12128, .F. ) ;
#1155 = FACE_OUTER_BOUND ( 'NONE', #3199, .T. ) ;
#1156 = CYLINDRICAL_SURFACE ( 'NONE', #8119, 1.500000000000000666 ) ;
#1157 = CIRCLE ( 'NONE', #15972, 1.500000000000000444 ) ;
#1158 = DIRECTION ( 'NONE',  ( -0.1566598588826321192, 0.9876526153536342445, 7.798540720466730171E-17 ) ) ;
#1159 = DIRECTION ( 'NONE',  ( -0.1566598588826321747, 0.9876526153536343555, 0.000000000000000000 ) ) ;
#1160 = DIRECTION ( 'NONE',  ( 1.000000000000000000, 0.000000000000000000, 0.000000000000000000 ) ) ;
#1161 = CARTESIAN_POINT ( 'NONE',  ( -128.1404785157144204, 9.631497293019437578, -2.500000000000000000 ) ) ;
#1162 = CIRCLE ( 'NONE', #11700, 145.0000000000000284 ) ;
#1163 = ORIENTED_EDGE ( 'NONE', *, *, #18121, .F. ) ;
#1164 = ORIENTED_EDGE ( 'NONE', *, *, #13310, .T. ) ;
#1165 = DIRECTION ( 'NONE',  ( -0.000000000000000000, -0.000000000000000000, 1.000000000000000000 ) ) ;
#1166 = EDGE_CURVE ( 'NONE', #17343, #6687, #1819, .T. ) ;
#1167 = EDGE_LOOP ( 'NONE', ( #16777, #1534 ) ) ;
#1168 = VERTEX_POINT ( 'NONE', #166 ) ;
#1169 = DIRECTION ( 'NONE',  ( -0.1566598588826321192, 0.9876526153536342445, 7.798540720466731404E-17 ) ) ;
#1170 = CIRCLE ( 'NONE', #9295, 2.000000000000000000 ) ;
#1171 = FACE_BOUND ( 'NONE', #8973, .T. ) ;
#1172 = EDGE_CURVE ( 'NONE', #8567, #13224, #4546, .T. ) ;
#1173 = EDGE_LOOP ( 'NONE', ( #13695, #16928, #14846, #15179 ) ) ;
#1174 = EDGE_LOOP ( 'NONE', ( #16625, #8138, #6275, #5012 ) ) ;
#1175 = AXIS2_PLACEMENT_3D ( 'NONE', #12005, #6274, #12108 ) ;
#1176 = ORIENTED_EDGE ( 'NONE', *, *, #5946, .T. ) ;
#1177 = ORIENTED_EDGE ( 'NONE', *, *, #3923, .F. ) ;
#1178 = AXIS2_PLACEMENT_3D ( 'NONE', #8807, #4352, #14496 ) ;
#1179 = CYLINDRICAL_SURFACE ( 'NONE', #6081, 1.500000000000001554 ) ;
#1180 = DIRECTION ( 'NONE',  ( -0.9876526153536341335, -0.1566598588826327021, 0.000000000000000000 ) ) ;
#1181 = LINE ( 'NONE', #16691, #8739 ) ;
#1182 = CIRCLE ( 'NONE', #3557, 1.500000000000000888 ) ;
#1183 = CIRCLE ( 'NONE', #6002, 1.499999999999999556 ) ;
#1184 = CARTESIAN_POINT ( 'NONE',  ( -90.00000000000000000, 34.99999999999999289, -2.499999999999974243 ) ) ;
#1185 = ORIENTED_EDGE ( 'NONE', *, *, #2912, .T. ) ;
#1187 = ORIENTED_EDGE ( 'NONE', *, *, #13997, .T. ) ;
#1186 = EDGE_CURVE ( 'NONE', #4810, #886, #3031, .T. ) ;
#1188 = VERTEX_POINT ( 'NONE', #12474 ) ;
#1189 = ORIENTED_EDGE ( 'NONE', *, *, #11793, .T. ) ;
#1190 = CARTESIAN_POINT ( 'NONE',  ( -4.361458684479201153, -15.87908452487173427, -17.32050807568878170 ) ) ;
#1191 = EDGE_CURVE ( 'NONE', #14798, #6605, #10294, .T. ) ;
#1192 = EDGE_CURVE ( 'NONE', #17282, #16734, #10892, .T. ) ;
#1193 = ORIENTED_EDGE ( 'NONE', *, *, #1553, .T. ) ;
#1194 = FACE_OUTER_BOUND ( 'NONE', #3187, .T. ) ;
#1195 = CARTESIAN_POINT ( 'NONE',  ( -77.40662104346073136, 32.93835651487657401, -35.00000000000000000 ) ) ;
#1196 = DIRECTION ( 'NONE',  ( -0.9876526153536336894, -0.1566598588826350336, 0.000000000000000000 ) ) ;
#1197 = VECTOR ( 'NONE', #3987, 1000.000000000000000 ) ;
#1198 = LINE ( 'NONE', #7160, #12742 ) ;
#1199 = VECTOR ( 'NONE', #745, 1000.000000000000000 ) ;
#1200 = AXIS2_PLACEMENT_3D ( 'NONE', #3723, #2696, #12829 ) ;
#1201 = DIRECTION ( 'NONE',  ( -0.9876526153536336894, -0.1566598588826350336, 0.000000000000000000 ) ) ;
#1202 = DIRECTION ( 'NONE',  ( -0.1566598588826321192, 0.9876526153536342445, 7.798540720466730171E-17 ) ) ;
#1203 = APPLICATION_PROTOCOL_DEFINITION ( 'draft international standard', 'automotive_design', 1998, #8103 ) ;
#1204 = FACE_OUTER_BOUND ( 'NONE', #1787, .T. ) ;
#1205 = DIRECTION ( 'NONE',  ( 0.000000000000000000, 0.000000000000000000, 1.000000000000000000 ) ) ;
#1206 = VECTOR ( 'NONE', #10253, 1000.000000000000000 ) ;
#1207 = CYLINDRICAL_SURFACE ( 'NONE', #7138, 1.500000000000000666 ) ;
#1208 = ORIENTED_EDGE ( 'NONE', *, *, #2727, .F. ) ;
#1209 = VERTEX_POINT ( 'NONE', #3546 ) ;
#1210 = CARTESIAN_POINT ( 'NONE',  ( -16.91146969734005268, -22.93225569655540141, -17.32050807568878170 ) ) ;
#1211 = CYLINDRICAL_SURFACE ( 'NONE', #2072, 20.00000000000001066 ) ;
#1212 = DIRECTION ( 'NONE',  ( -0.1566598588826321192, 0.9876526153536342445, 7.798540720466730171E-17 ) ) ;
#1213 = AXIS2_PLACEMENT_3D ( 'NONE', #10785, #16709, #13826 ) ;
#1214 = EDGE_CURVE ( 'NONE', #13600, #3308, #2125, .T. ) ;
#1215 = LINE ( 'NONE', #7000, #4553 ) ;
#1216 = AXIS2_PLACEMENT_3D ( 'NONE', #2129, #13678, #3527 ) ;
#1217 = ORIENTED_EDGE ( 'NONE', *, *, #18525, .F. ) ;
#1218 = FACE_OUTER_BOUND ( 'NONE', #3277, .T. ) ;
#1219 = DIRECTION ( 'NONE',  ( -0.9876526153536341335, -0.1566598588826327021, 0.000000000000000000 ) ) ;
#1220 = ADVANCED_FACE ( 'NONE', ( #9641 ), #2329, .T. ) ;
#1221 = AXIS2_PLACEMENT_3D ( 'NONE', #5833, #7158, #8480 ) ;
#1222 = LINE ( 'NONE', #12750, #18237 ) ;
#1223 = EDGE_CURVE ( 'NONE', #12973, #12986, #9398, .T. ) ;
#1224 = DIRECTION ( 'NONE',  ( -0.9876526153536341335, -0.1566598588826327021, 0.000000000000000000 ) ) ;
#1225 = VECTOR ( 'NONE', #12033, 1000.000000000000000 ) ;
#1226 = CARTESIAN_POINT ( 'NONE',  ( -10.98555400521827607, -21.99229654325962002, 4.330127018922214077 ) ) ;
#1227 = CIRCLE ( 'NONE', #16352, 12.74754878398197633 ) ;
#1228 = DIRECTION ( 'NONE',  ( -0.9876526153536336894, -0.1566598588826349503, 0.000000000000000000 ) ) ;
#1229 = CIRCLE ( 'NONE', #15424, 1.500000000000000888 ) ;
#1230 = CARTESIAN_POINT ( 'NONE',  ( -83.14047854185180597, 6.938893903907228378E-15, 25.00000000000002132 ) ) ;
#1231 = LINE ( 'NONE', #7109, #13735 ) ;
#1232 = DIRECTION ( 'NONE',  ( -0.1566598588826321747, 0.9876526153536343555, 0.000000000000000000 ) ) ;
#1233 = VERTEX_POINT ( 'NONE', #9452 ) ;
#1234 = DIRECTION ( 'NONE',  ( 0.9876526153536341335, -0.1566598588826326743, 0.000000000000000000 ) ) ;
#1235 = CARTESIAN_POINT ( 'NONE',  ( -70.00000000000000000, 44.99999999999999289, 20.00000000000001776 ) ) ;
#1237 = ORIENTED_EDGE ( 'NONE', *, *, #1546, .T. ) ;
#1236 = DIRECTION ( 'NONE',  ( -0.1566598588826321192, 0.9876526153536342445, 7.798540720466730171E-17 ) ) ;
#1238 = AXIS2_PLACEMENT_3D ( 'NONE', #16759, #16849, #17042 ) ;
#1239 = CARTESIAN_POINT ( 'NONE',  ( -43.08426400421126345, -27.08374195694514341, -8.660254037844380193 ) ) ;
#1240 = CIRCLE ( 'NONE', #3302, 1.500000000000001332 ) ;
#1241 = EDGE_LOOP ( 'NONE', ( #7462, #12015, #9169, #11444 ) ) ;
#1242 = CIRCLE ( 'NONE', #3928, 1.500000000000000000 ) ;
#1243 = DIRECTION ( 'NONE',  ( -0.1566598588826321192, 0.9876526153536342445, 7.798540720466730171E-17 ) ) ;
#1244 = EDGE_CURVE ( 'NONE', #403, #16695, #13918, .T. ) ;
#1245 = CARTESIAN_POINT ( 'NONE',  ( -110.7369027592740167, -34.07064978273316314, -2.500000000000000000 ) ) ;
#1246 = EDGE_CURVE ( 'NONE', #4660, #13845, #12174, .T. ) ;
#1247 = LINE ( 'NONE', #7032, #4023 ) ;
#1248 = DIRECTION ( 'NONE',  ( -0.9876526153536341335, -0.1566598588826327021, 0.000000000000000000 ) ) ;
#1249 = DIRECTION ( 'NONE',  ( -0.1566598588826321192, 0.9876526153536342445, 7.798540720466730171E-17 ) ) ;
#1250 = AXIS2_PLACEMENT_3D ( 'NONE', #12266, #18216, #3736 ) ;
#1251 = ADVANCED_FACE ( 'NONE', ( #2439 ), #8122, .F. ) ;
#1252 = DIRECTION ( 'NONE',  ( -0.9876526153536336894, -0.1566598588826350336, 0.000000000000000000 ) ) ;
#1253 = DIRECTION ( 'NONE',  ( -0.9876526153536336894, -0.1566598588826350336, 0.000000000000000000 ) ) ;
#1254 = AXIS2_PLACEMENT_3D ( 'NONE', #14338, #15644, #15845 ) ;
#1255 = DIRECTION ( 'NONE',  ( -2.735665993912342121E-16, -0.000000000000000000, -1.000000000000000000 ) ) ;
#1256 = VECTOR ( 'NONE', #2851, 1000.000000000000000 ) ;
#1257 = AXIS2_PLACEMENT_3D ( 'NONE', #12290, #9196, #14966 ) ;
#1258 = ORIENTED_EDGE ( 'NONE', *, *, #6088, .F. ) ;
#1259 = AXIS2_PLACEMENT_3D ( 'NONE', #4319, #2972, #15878 ) ;
#1260 = EDGE_LOOP ( 'NONE', ( #9417, #10495, #17087, #8009 ) ) ;
#1261 = EDGE_LOOP ( 'NONE', ( #16723, #9900, #18731, #3471, #10997, #3485 ) ) ;
#1262 = CARTESIAN_POINT ( 'NONE',  ( -170.4124675745486570, 31.54971992778987655, 2.500000000000000000 ) ) ;
#1263 = VERTEX_POINT ( 'NONE', #9253 ) ;
#1264 = VERTEX_POINT ( 'NONE', #7940 ) ;
#1265 = VERTEX_POINT ( 'NONE', #18401 ) ;
#1266 = CIRCLE ( 'NONE', #12101, 2.000000000000000000 ) ;
#1267 = VERTEX_POINT ( 'NONE', #12552 ) ;
#1268 = FACE_OUTER_BOUND ( 'NONE', #14639, .T. ) ;
#1269 = CIRCLE ( 'NONE', #13322, 1.500000000000000444 ) ;
#1270 = CARTESIAN_POINT ( 'NONE',  ( -24.27922930231443743, -81.80638607452326028, -8.660254037844385522 ) ) ;
#1271 = CARTESIAN_POINT ( 'NONE',  ( -23.12685837619818940, -18.85562184364173888, -12.99038105676658006 ) ) ;
#1272 = ORIENTED_EDGE ( 'NONE', *, *, #9509, .T. ) ;
#1273 = ADVANCED_FACE ( 'NONE', ( #6720 ), #18309, .F. ) ;
#1274 = CARTESIAN_POINT ( 'NONE',  ( -129.1404785418517918, 9.649298036820672664, 2.500000000000000000 ) ) ;
#1275 = ORIENTED_EDGE ( 'NONE', *, *, #17968, .T. ) ;
#1276 = CIRCLE ( 'NONE', #7029, 2.000000000000000000 ) ;
#1277 = CIRCLE ( 'NONE', #11817, 1.500000000000000888 ) ;
#1278 = CARTESIAN_POINT ( 'NONE',  ( -1.069392841504132052, -78.12487939078141608, 1.077796531449093893E-14 ) ) ;
#1279 = CARTESIAN_POINT ( 'NONE',  ( -5.349111299832828514, -16.03574438375436984, -4.330127018922183879 ) ) ;
#1281 = ADVANCED_FACE ( 'NONE', ( #16473 ), #649, .F. ) ;
#1280 = CARTESIAN_POINT ( 'NONE',  ( -344.2740538294495423, -1.635550152012466452, 9.951701414186830458E-16 ) ) ;
#1282 = FACE_BOUND ( 'NONE', #11132, .T. ) ;
#1283 = FACE_OUTER_BOUND ( 'NONE', #17126, .T. ) ;
#1284 = AXIS2_PLACEMENT_3D ( 'NONE', #8706, #1338, #15827 ) ;
#1285 = ORIENTED_EDGE ( 'NONE', *, *, #16091, .T. ) ;
#1286 = ORIENTED_EDGE ( 'NONE', *, *, #15705, .F. ) ;
#1287 = DIRECTION ( 'NONE',  ( 0.000000000000000000, 0.000000000000000000, 1.000000000000000000 ) ) ;
#1288 = EDGE_LOOP ( 'NONE', ( #2095, #8493, #3511, #9093 ) ) ;
#1289 = CARTESIAN_POINT ( 'NONE',  ( 2.058283315319403783, -14.86079544213463066, -17.32050807568878170 ) ) ;
#1290 = VECTOR ( 'NONE', #2283, 1000.000000000000000 ) ;
#1291 = DIRECTION ( 'NONE',  ( -0.1566598588826321192, 0.9876526153536342445, 7.798540720466730171E-17 ) ) ;
#1292 = EDGE_LOOP ( 'NONE', ( #10578, #3990 ) ) ;
#1293 = AXIS2_PLACEMENT_3D ( 'NONE', #3370, #9175, #14945 ) ;
#1294 = DIRECTION ( 'NONE',  ( 1.000000000000000000, 0.000000000000000000, 0.000000000000000000 ) ) ;
#1295 = DIRECTION ( 'NONE',  ( 1.000000000000000000, 0.000000000000000000, 0.000000000000000000 ) ) ;
#1296 = AXIS2_PLACEMENT_3D ( 'NONE', #1979, #17943, #8906 ) ;
#1297 = EDGE_CURVE ( 'NONE', #6069, #14627, #17290, .T. ) ;
#1298 = EDGE_CURVE ( 'NONE', #5533, #356, #10749, .T. ) ;
#1299 = CARTESIAN_POINT ( 'NONE',  ( -174.8673125818257006, 55.13264502119463373, 5.500000000000001776 ) ) ;
#1300 = DIRECTION ( 'NONE',  ( 0.000000000000000000, 0.000000000000000000, 1.000000000000000000 ) ) ;
#1302 = ADVANCED_FACE ( 'NONE', ( #6615 ), #5188, .F. ) ;
#1301 = CARTESIAN_POINT ( 'NONE',  ( -0.9046745307415022808, -15.33077501878252136, 17.32050807568881012 ) ) ;
#1303 = CARTESIAN_POINT ( 'NONE',  ( 6.744699544032231168E-15, -6.824871242521816123E-15, 20.00000000000000000 ) ) ;
#1304 = ORIENTED_EDGE ( 'NONE', *, *, #16796, .T. ) ;
#1305 = EDGE_LOOP ( 'NONE', ( #4565, #16384, #1189, #9828 ) ) ;
#1306 = CARTESIAN_POINT ( 'NONE',  ( -69.25705831108246002, -31.23522821733487476, 1.869203119972154228E-14 ) ) ;
#1307 = CARTESIAN_POINT ( 'NONE',  ( 59.44021041145193607, -44.12097743988038445, 19.99999999999998579 ) ) ;
#1308 = FACE_OUTER_BOUND ( 'NONE', #11877, .T. ) ;
#1309 = ORIENTED_EDGE ( 'NONE', *, *, #1355, .F. ) ;
#1310 = ORIENTED_EDGE ( 'NONE', *, *, #3150, .F. ) ;
#1311 = CYLINDRICAL_SURFACE ( 'NONE', #648, 2.000000000000001776 ) ;
#1312 = VERTEX_POINT ( 'NONE', #13991 ) ;
#1313 = CARTESIAN_POINT ( 'NONE',  ( -61.35583738825340561, -29.98194934627382224, 1.887572821959364500E-14 ) ) ;
#1314 = VERTEX_POINT ( 'NONE', #6522 ) ;
#1315 = CARTESIAN_POINT ( 'NONE',  ( -40.61513246582718040, -26.69209230973856251, 4.330127018922217630 ) ) ;
#1316 = DIRECTION ( 'NONE',  ( -0.000000000000000000, -0.000000000000000000, -1.000000000000000000 ) ) ;
#1317 = FILL_AREA_STYLE ('',( #8512 ) ) ;
#1318 = ORIENTED_EDGE ( 'NONE', *, *, #11898, .T. ) ;
#1319 = EDGE_CURVE ( 'NONE', #2695, #14517, #15220, .T. ) ;
#1320 = CIRCLE ( 'NONE', #17676, 1.500000000000000888 ) ;
#1321 = DIRECTION ( 'NONE',  ( -0.9876526153536336894, -0.1566598588826349503, 0.000000000000000000 ) ) ;
#1322 = CARTESIAN_POINT ( 'NONE',  ( -20.82244514857674389, -81.25807656843406335, 17.32050807568881368 ) ) ;
#1323 = LINE ( 'NONE', #14293, #16494 ) ;
#1324 = DIRECTION ( 'NONE',  ( -0.1566598588826321192, 0.9876526153536342445, 7.798540720466730171E-17 ) ) ;
#1325 = EDGE_LOOP ( 'NONE', ( #11302, #17504, #9683, #6379 ) ) ;
#1326 = VERTEX_POINT ( 'NONE', #17336 ) ;
#1327 = ADVANCED_FACE ( 'NONE', ( #12844 ), #15591, .F. ) ;
#1328 = CARTESIAN_POINT ( 'NONE',  ( -33.16810284049710589, -83.21632480446696434, 4.330127018922213189 ) ) ;
#1329 = ORIENTED_EDGE ( 'NONE', *, *, #690, .T. ) ;
#1330 = EDGE_CURVE ( 'NONE', #4398, #10018, #12723, .T. ) ;
#1331 = EDGE_CURVE ( 'NONE', #7954, #16292, #18686, .T. ) ;
#1332 = DIRECTION ( 'NONE',  ( -0.9876526153536336894, -0.1566598588826349503, 0.000000000000000000 ) ) ;
#1333 = ORIENTED_EDGE ( 'NONE', *, *, #13285, .T. ) ;
#1334 = AXIS2_PLACEMENT_3D ( 'NONE', #11257, #3005, #8795 ) ;
#1335 = DIRECTION ( 'NONE',  ( -0.9876526153536341335, -0.1566598588826327021, 0.000000000000000000 ) ) ;
#1336 = DIRECTION ( 'NONE',  ( -0.1566598588826321192, 0.9876526153536342445, 7.798540720466731404E-17 ) ) ;
#1337 = CARTESIAN_POINT ( 'NONE',  ( 73.09088021254186174, 1.387778780781445676E-14, 19.99999999999997513 ) ) ;
#1338 = DIRECTION ( 'NONE',  ( -0.1566598588826321747, 0.9876526153536343555, 0.000000000000000000 ) ) ;
#1339 = DIRECTION ( 'NONE',  ( -0.3915338189555019333, 0.9201637183752250371, 0.000000000000000000 ) ) ;
#1340 = CARTESIAN_POINT ( 'NONE',  ( 11.59211860341526723, 6.314490184041260612, -20.00000000000000355 ) ) ;
#1341 = FACE_OUTER_BOUND ( 'NONE', #6254, .T. ) ;
#1342 = DIRECTION ( 'NONE',  ( 0.000000000000000000, 0.000000000000000000, 1.000000000000000000 ) ) ;
#1343 = FACE_BOUND ( 'NONE', #4982, .T. ) ;
#1344 = PLANE ( 'NONE',  #13494 ) ;
#1345 = CARTESIAN_POINT ( 'NONE',  ( -45.55339554259533230, -27.47539160415171722, -12.99038105676658006 ) ) ;
#1346 = VECTOR ( 'NONE', #12553, 1000.000000000000000 ) ;
#1348 = EDGE_LOOP ( 'NONE', ( #7266, #4707, #14572, #15451 ) ) ;
#1347 = CARTESIAN_POINT ( 'NONE',  ( -90.00000000000000000, 34.99999999999999289, -30.00000000000000000 ) ) ;
#1349 = EDGE_CURVE ( 'NONE', #4102, #15920, #6693, .T. ) ;
#1350 = EDGE_CURVE ( 'NONE', #16790, #17286, #5177, .T. ) ;
#1351 = FACE_OUTER_BOUND ( 'NONE', #7199, .T. ) ;
#1352 = ORIENTED_EDGE ( 'NONE', *, *, #4629, .T. ) ;
#1353 = ORIENTED_EDGE ( 'NONE', *, *, #315, .F. ) ;
#1354 = CARTESIAN_POINT ( 'NONE',  ( 0.000000000000000000, 0.000000000000000000, -35.00000000000000000 ) ) ;
#1355 = EDGE_CURVE ( 'NONE', #13473, #12774, #14782, .T. ) ;
#1356 = CYLINDRICAL_SURFACE ( 'NONE', #8842, 2.500000000000002220 ) ;
#1357 = DIRECTION ( 'NONE',  ( -0.1566598588826321747, 0.9876526153536343555, 0.000000000000000000 ) ) ;
#1358 = LINE ( 'NONE', #8913, #6063 ) ;
#1359 = CARTESIAN_POINT ( 'NONE',  ( -2.200000000000000178, 0.000000000000000000, -19.99999999999999645 ) ) ;
#1360 = ORIENTED_EDGE ( 'NONE', *, *, #12905, .F. ) ;
#1361 = FACE_BOUND ( 'NONE', #17500, .T. ) ;
#1362 = CARTESIAN_POINT ( 'NONE',  ( -20.32861884089991023, -81.17974663899271093, -21.65063509461098690 ) ) ;
#1363 = CARTESIAN_POINT ( 'NONE',  ( -90.00000000000000000, 34.99999999999999289, -30.00000000000000000 ) ) ;
#1364 = CARTESIAN_POINT ( 'NONE',  ( -126.1404785418517918, 6.938893903907228378E-15, 5.500000000000000000 ) ) ;
#1365 = FACE_OUTER_BOUND ( 'NONE', #18646, .T. ) ;
#1366 = ORIENTED_EDGE ( 'NONE', *, *, #4171, .T. ) ;
#1367 = DIRECTION ( 'NONE',  ( -0.9876526153536341335, -0.1566598588826327021, 0.000000000000000000 ) ) ;
#1368 = EDGE_LOOP ( 'NONE', ( #7951, #8946, #1833, #12084 ) ) ;
#1369 = VERTEX_POINT ( 'NONE', #1398 ) ;
#1370 = ORIENTED_EDGE ( 'NONE', *, *, #15991, .T. ) ;
#1371 = DIRECTION ( 'NONE',  ( 0.000000000000000000, 0.000000000000000000, 1.000000000000000000 ) ) ;
#1372 = EDGE_CURVE ( 'NONE', #2469, #4280, #4254, .T. ) ;
#1373 = AXIS2_PLACEMENT_3D ( 'NONE', #9286, #3128, #11730 ) ;
#1374 = FACE_BOUND ( 'NONE', #314, .T. ) ;
#1375 = CYLINDRICAL_SURFACE ( 'NONE', #1221, 1.500000000000001554 ) ;
#1376 = ORIENTED_EDGE ( 'NONE', *, *, #4127, .T. ) ;
#1377 = EDGE_CURVE ( 'NONE', #14160, #10171, #17137, .T. ) ;
#1378 = DIRECTION ( 'NONE',  ( -0.1566598588826321192, 0.9876526153536342445, 7.798540720466730171E-17 ) ) ;
#1379 = ADVANCED_FACE ( 'NONE', ( #9748 ), #4322, .F. ) ;
#1380 = FACE_OUTER_BOUND ( 'NONE', #4464, .T. ) ;
#1381 = ITEM_DEFINED_TRANSFORMATION ( 'NONE', 'NONE', #6295,  #18772 ) ;
#1382 = EDGE_LOOP ( 'NONE', ( #4177, #17416 ) ) ;
#1383 = CARTESIAN_POINT ( 'NONE',  ( -49.59961335071797350, 39.40051552679457814, -130.3485206753969976 ) ) ;
#1384 = CARTESIAN_POINT ( 'NONE',  ( -79.23462711737164454, 33.01666666666666572, 35.00000000000000000 ) ) ;
#1385 = DIRECTION ( 'NONE',  ( 0.000000000000000000, 0.000000000000000000, -1.000000000000000000 ) ) ;
#1386 = FACE_OUTER_BOUND ( 'NONE', #16373, .T. ) ;
#1387 = ORIENTED_EDGE ( 'NONE', *, *, #3448, .T. ) ;
#1388 = ORIENTED_EDGE ( 'NONE', *, *, #7142, .T. ) ;
#1389 = FACE_BOUND ( 'NONE', #17368, .T. ) ;
#1390 = DIRECTION ( 'NONE',  ( -0.1566598588826321192, 0.9876526153536342445, 7.798540720466730171E-17 ) ) ;
#1391 = CARTESIAN_POINT ( 'NONE',  ( -67.07739975943471222, -25.82698556391885347, -8.660254037844380193 ) ) ;
#1392 = ORIENTED_EDGE ( 'NONE', *, *, #17578, .F. ) ;
#1393 = CARTESIAN_POINT ( 'NONE',  ( -175.0529311237955596, 56.11526690008648899, 2.500000000000000000 ) ) ;
#1394 = EDGE_CURVE ( 'NONE', #2218, #14954, #1266, .T. ) ;
#1395 = CIRCLE ( 'NONE', #176, 1.500000000000000888 ) ;
#1396 = DIRECTION ( 'NONE',  ( -0.1566598588826321747, 0.9876526153536343555, 0.000000000000000000 ) ) ;
#1397 = ADVANCED_FACE ( 'NONE', ( #13031 ), #4562, .T. ) ;
#1398 = CARTESIAN_POINT ( 'NONE',  ( -69.54653129781877396, -26.21863521112543793, 4.330127018922218518 ) ) ;
#1399 = DIRECTION ( 'NONE',  ( 0.000000000000000000, 0.000000000000000000, 1.000000000000000000 ) ) ;
#1400 = DIRECTION ( 'NONE',  ( 0.9876526153536342445, 0.1566598588826321470, 0.000000000000000000 ) ) ;
#1401 = CIRCLE ( 'NONE', #5634, 1.500000000000000000 ) ;
#1402 = DIRECTION ( 'NONE',  ( -0.9876526153536341335, -0.1566598588826327021, 0.000000000000000000 ) ) ;
#1403 = ORIENTED_EDGE ( 'NONE', *, *, #6674, .F. ) ;
#1404 = DIRECTION ( 'NONE',  ( -0.9876526153536336894, -0.1566598588826349503, 0.000000000000000000 ) ) ;
#1405 = FACE_OUTER_BOUND ( 'NONE', #1455, .T. ) ;
#1406 = DIRECTION ( 'NONE',  ( -0.1566598588826321192, 0.9876526153536342445, 7.798540720466730171E-17 ) ) ;
#1407 = ORIENTED_EDGE ( 'NONE', *, *, #18253, .F. ) ;
#1408 = CARTESIAN_POINT ( 'NONE',  ( -60.36818477289978091, -29.82528948739120267, -21.65063509461098334 ) ) ;
#1410 = ORIENTED_EDGE ( 'NONE', *, *, #11519, .F. ) ;
#1409 = CARTESIAN_POINT ( 'NONE',  ( -170.4124675745486570, 31.54971992778987655, -2.500000000000000000 ) ) ;
#1411 = EDGE_CURVE ( 'NONE', #13426, #11861, #9725, .T. ) ;
#1412 = ORIENTED_EDGE ( 'NONE', *, *, #10407, .F. ) ;
#1413 = DIRECTION ( 'NONE',  ( -0.9876526153536341335, -0.1566598588826327576, 0.000000000000000000 ) ) ;
#1414 = LINE ( 'NONE', #12945, #627 ) ;
#1415 = VERTEX_POINT ( 'NONE', #14181 ) ;
#1416 = EDGE_LOOP ( 'NONE', ( #18088, #13081 ) ) ;
#1417 = EDGE_CURVE ( 'NONE', #1906, #5889, #1222, .T. ) ;
#1418 = ADVANCED_FACE ( 'NONE', ( #14734 ), #10459, .F. ) ;
#1419 = EDGE_CURVE ( 'NONE', #7156, #16655, #7895, .T. ) ;
#1420 = CIRCLE ( 'NONE', #11676, 1.500000000000000888 ) ;
#1421 = LINE ( 'NONE', #7117, #670 ) ;
#1422 = CARTESIAN_POINT ( 'NONE',  ( -33.99103714508810725, -20.57888029135069274, 1.908195823574487804E-14 ) ) ;
#1423 = CARTESIAN_POINT ( 'NONE',  ( -16.91146969734005268, -22.93225569655540141, 17.32050807568881012 ) ) ;
#1424 = VECTOR ( 'NONE', #5665, 1000.000000000000000 ) ;
#1425 = DIRECTION ( 'NONE',  ( -0.9876526153536341335, -0.1566598588826327021, 0.000000000000000000 ) ) ;
#1426 = DIRECTION ( 'NONE',  ( -0.1566598588826321192, 0.9876526153536342445, 7.798540720466730171E-17 ) ) ;
#1427 = CARTESIAN_POINT ( 'NONE',  ( -61.31620237807555895, -87.68113078262194904, 4.330127018922213189 ) ) ;
#1428 = DIRECTION ( 'NONE',  ( 0.000000000000000000, 0.000000000000000000, 1.000000000000000000 ) ) ;
#1429 = CARTESIAN_POINT ( 'NONE',  ( -20.65772683781411345, -18.46397219643516152, -8.660254037844380193 ) ) ;
#1430 = FACE_BOUND ( 'NONE', #6889, .T. ) ;
#1431 = LINE ( 'NONE', #4433, #16913 ) ;
#1432 = VECTOR ( 'NONE', #11631, 1000.000000000000000 ) ;
#1434 = ORIENTED_EDGE ( 'NONE', *, *, #11049, .T. ) ;
#1433 = CARTESIAN_POINT ( 'NONE',  ( -68.55887868246516348, -26.06197535224280415, 8.660254037844417496 ) ) ;
#1435 = CARTESIAN_POINT ( 'NONE',  ( -2.590506774712417748, -20.66068774275724707, 4.330127018922212301 ) ) ;
#1436 = VERTEX_POINT ( 'NONE', #16251 ) ;
#1437 = CIRCLE ( 'NONE', #6282, 1.500000000000001332 ) ;
#1438 = EDGE_LOOP ( 'NONE', ( #17360, #14146 ) ) ;
#1439 = DIRECTION ( 'NONE',  ( -0.9876526153536336894, -0.1566598588826349503, 0.000000000000000000 ) ) ;
#1440 = AXIS2_PLACEMENT_3D ( 'NONE', #10747, #3544, #16857 ) ;
#1441 = FACE_BOUND ( 'NONE', #12061, .T. ) ;
#1442 = CIRCLE ( 'NONE', #14123, 1.499999999999999556 ) ;
#1443 = CARTESIAN_POINT ( 'NONE',  ( -25.80034323552273534, -24.34219442649909126, 21.65063509461101887 ) ) ;
#1444 = EDGE_CURVE ( 'NONE', #11927, #13075, #13931, .T. ) ;
#1445 = ADVANCED_BREP_SHAPE_REPRESENTATION ( '', ( #8651, #18772 ), #13228 ) ;
#1446 = EDGE_CURVE ( 'NONE', #13518, #9479, #18546, .T. ) ;
#1447 = AXIS2_PLACEMENT_3D ( 'NONE', #18670, #137, #1205 ) ;
#1448 = CIRCLE ( 'NONE', #18120, 1.500000000000001332 ) ;
#1449 = CARTESIAN_POINT ( 'NONE',  ( -52.75643683680706886, -23.55541761012069912, 12.99038105676661736 ) ) ;
#1450 = DIRECTION ( 'NONE',  ( -0.1566598588826321747, 0.9876526153536343555, 0.000000000000000000 ) ) ;
#1451 = DIRECTION ( 'NONE',  ( -0.1566598588826321192, 0.9876526153536342445, 7.798540720466730171E-17 ) ) ;
#1452 = FACE_BOUND ( 'NONE', #7236, .T. ) ;
#1453 = CARTESIAN_POINT ( 'NONE',  ( -63.62061560569701157, -25.27867605782964233, 1.908195823574487804E-14 ) ) ;
#1454 = ORIENTED_EDGE ( 'NONE', *, *, #1350, .T. ) ;
#1455 = EDGE_LOOP ( 'NONE', ( #13094, #13490 ) ) ;
#1456 = VERTEX_POINT ( 'NONE', #11600 ) ;
#1457 = VERTEX_POINT ( 'NONE', #3078 ) ;
#1458 = DIRECTION ( 'NONE',  ( -0.9876526153536341335, -0.1566598588826327021, 0.000000000000000000 ) ) ;
#1459 = VERTEX_POINT ( 'NONE', #17619 ) ;
#1460 = DIRECTION ( 'NONE',  ( -0.1566598588826321192, 0.9876526153536342445, 7.798540720466730171E-17 ) ) ;
#1461 = AXIS2_PLACEMENT_3D ( 'NONE', #12294, #7961, #14881 ) ;
#1462 = DIRECTION ( 'NONE',  ( 2.887450008416415878E-16, 0.000000000000000000, 1.000000000000000000 ) ) ;
#1463 = ORIENTED_EDGE ( 'NONE', *, *, #11826, .F. ) ;
#1464 = LINE ( 'NONE', #11580, #10011 ) ;
#1465 = EDGE_CURVE ( 'NONE', #5203, #17378, #14844, .T. ) ;
#1466 = AXIS2_PLACEMENT_3D ( 'NONE', #18717, #11166, #16991 ) ;
#1467 = DIRECTION ( 'NONE',  ( -0.9876526153536341335, 0.1566598588826326743, 2.851797552515345870E-16 ) ) ;
#1468 = LINE ( 'NONE', #11581, #8547 ) ;
#1469 = APPLICATION_PROTOCOL_DEFINITION ( 'draft international standard', 'automotive_design', 1998, #7500 ) ;
#1470 = CIRCLE ( 'NONE', #14176, 1.500000000000001332 ) ;
#1471 = EDGE_CURVE ( 'NONE', #4101, #8059, #13631, .T. ) ;
#1472 = DIRECTION ( 'NONE',  ( -0.9876526153536336894, -0.1566598588826349503, 0.000000000000000000 ) ) ;
#1473 = DIRECTION ( 'NONE',  ( 1.000000000000000000, 0.000000000000000000, 0.000000000000000000 ) ) ;
#1474 =( LENGTH_UNIT ( ) NAMED_UNIT ( * ) SI_UNIT ( .MILLI., .METRE. ) );
#1475 = CARTESIAN_POINT ( 'NONE',  ( -70.24339520416560845, 45.10356575889633746, -5.890567936347699707 ) ) ;
#1476 = ORIENTED_EDGE ( 'NONE', *, *, #6473, .T. ) ;
#1477 = VERTEX_POINT ( 'NONE', #10557 ) ;
#1478 = CARTESIAN_POINT ( 'NONE',  ( -36.62488699423479943, -83.76463431055617548, 21.65063509461101532 ) ) ;
#1479 = CARTESIAN_POINT ( 'NONE',  ( -17.85948730251583783, -80.78809699178616199, 17.32050807568881368 ) ) ;
#1480 = EDGE_CURVE ( 'NONE', #5250, #15378, #9096, .T. ) ;
#1481 = DIRECTION ( 'NONE',  ( 0.9876526153536342445, 0.1566598588826321470, 0.000000000000000000 ) ) ;
#1482 = ORIENTED_EDGE ( 'NONE', *, *, #2611, .F. ) ;
#1483 = DIRECTION ( 'NONE',  ( -0.000000000000000000, -0.000000000000000000, -1.000000000000000000 ) ) ;
#1484 = DIRECTION ( 'NONE',  ( -0.1566598588826321192, 0.9876526153536342445, 7.798540720466730171E-17 ) ) ;
#1485 = AXIS2_PLACEMENT_3D ( 'NONE', #7363, #4399, #17328 ) ;
#1486 = EDGE_LOOP ( 'NONE', ( #6896, #992 ) ) ;
#1487 = CARTESIAN_POINT ( 'NONE',  ( -126.1404785418517918, -15.29729532696464922, 2.500000000000000000 ) ) ;
#1488 = CIRCLE ( 'NONE', #8142, 1.500000000000000888 ) ;
#1489 = VECTOR ( 'NONE', #5333, 1000.000000000000000 ) ;
#1490 = DIRECTION ( 'NONE',  ( 0.000000000000000000, 0.000000000000000000, 1.000000000000000000 ) ) ;
#1491 = CARTESIAN_POINT ( 'NONE',  ( -58.68235252892885256, -24.49537676341648762, 8.660254037844417496 ) ) ;
#1492 = DIRECTION ( 'NONE',  ( -1.000000000000000000, 0.000000000000000000, 0.000000000000000000 ) ) ;
#1493 = AXIS2_PLACEMENT_3D ( 'NONE', #14628, #11848, #16229 ) ;
#1494 = EDGE_CURVE ( 'NONE', #13776, #10500, #13396, .T. ) ;
#1495 = FACE_OUTER_BOUND ( 'NONE', #799, .T. ) ;
#1497 = DIRECTION ( 'NONE',  ( -0.1566598588826321192, 0.9876526153536342445, 7.798540720466730171E-17 ) ) ;
#1496 = CIRCLE ( 'NONE', #3568, 1.500000000000000888 ) ;
#1498 = LINE ( 'NONE', #13038, #17120 ) ;
#1499 = CIRCLE ( 'NONE', #16019, 1.500000000000000888 ) ;
#1500 = ORIENTED_EDGE ( 'NONE', *, *, #14501, .F. ) ;
#1501 = DIRECTION ( 'NONE',  ( -0.9876526153536341335, -0.1566598588826327021, 0.000000000000000000 ) ) ;
#1502 = AXIS2_PLACEMENT_3D ( 'NONE', #17737, #4711, #268 ) ;
#1504 = EDGE_LOOP ( 'NONE', ( #15054, #14543, #13451, #4712 ) ) ;
#1503 = LINE ( 'NONE', #79, #9060 ) ;
#1505 = EDGE_CURVE ( 'NONE', #12166, #3971, #8871, .T. ) ;
#1506 = VERTEX_POINT ( 'NONE', #6219 ) ;
#1507 = CYLINDRICAL_SURFACE ( 'NONE', #318, 1.500000000000001554 ) ;
#1508 = ORIENTED_EDGE ( 'NONE', *, *, #17437, .T. ) ;
#1509 = CIRCLE ( 'NONE', #599, 1.500000000000000888 ) ;
#1510 = AXIS2_PLACEMENT_3D ( 'NONE', #7878, #10979, #7968 ) ;
#1511 = DIRECTION ( 'NONE',  ( -0.000000000000000000, -0.000000000000000000, -1.000000000000000000 ) ) ;
#1512 = ORIENTED_EDGE ( 'NONE', *, *, #14379, .F. ) ;
#1513 = AXIS2_PLACEMENT_3D ( 'NONE', #9646, #10955, #3741 ) ;
#1514 = DIRECTION ( 'NONE',  ( 0.000000000000000000, 0.000000000000000000, 1.000000000000000000 ) ) ;
#1515 = DIRECTION ( 'NONE',  ( -2.671473304378624222E-16, -0.000000000000000000, -1.000000000000000000 ) ) ;
#1516 = AXIS2_PLACEMENT_3D ( 'NONE', #17367, #14497, #8629 ) ;
#1517 = CARTESIAN_POINT ( 'NONE',  ( -52.96079015774756016, -28.65034054577145994, 1.869203119972154228E-14 ) ) ;
#1518 = LINE ( 'NONE', #10207, #13241 ) ;
#1519 = CARTESIAN_POINT ( 'NONE',  ( -306.0881213225399051, -2.850701963179328668, 9.951701414186818625E-16 ) ) ;
#1520 = DIRECTION ( 'NONE',  ( -0.1566598588826321192, 0.9876526153536342445, 7.798540720466731404E-17 ) ) ;
#1521 = FACE_BOUND ( 'NONE', #3260, .T. ) ;
#1522 = EDGE_CURVE ( 'NONE', #334, #10470, #16170, .T. ) ;
#1523 = CYLINDRICAL_SURFACE ( 'NONE', #16034, 2.000000000000000000 ) ;
#1524 = EDGE_CURVE ( 'NONE', #15683, #6731, #16690, .T. ) ;
#1525 = CIRCLE ( 'NONE', #11179, 18.88854657239857815 ) ;
#1526 = EDGE_LOOP ( 'NONE', ( #6897, #6518, #14749, #5534 ) ) ;
#1527 = ADVANCED_FACE ( 'NONE', ( #13477 ), #6129, .T. ) ;
#1528 = AXIS2_PLACEMENT_3D ( 'NONE', #12056, #1946, #15210 ) ;
#1529 = ORIENTED_EDGE ( 'NONE', *, *, #4633, .T. ) ;
#1530 = DIRECTION ( 'NONE',  ( -0.9876526153536336894, -0.1566598588826349503, 0.000000000000000000 ) ) ;
#1531 = AXIS2_PLACEMENT_3D ( 'NONE', #6549, #3301, #3484 ) ;
#1532 = VERTEX_POINT ( 'NONE', #9047 ) ;
#1533 = PRODUCT_DEFINITION ( 'UNKNOWN', '', #3845, #2079 ) ;
#1534 = ORIENTED_EDGE ( 'NONE', *, *, #13160, .T. ) ;
#1535 = DIRECTION ( 'NONE',  ( -0.1566598588826321747, 0.9876526153536343555, 0.000000000000000000 ) ) ;
#1536 = FACE_BOUND ( 'NONE', #12481, .T. ) ;
#1537 = ORIENTED_EDGE ( 'NONE', *, *, #16319, .T. ) ;
#1538 = CIRCLE ( 'NONE', #934, 1.500000000000000444 ) ;
#1539 = CARTESIAN_POINT ( 'NONE',  ( -76.95187462163347902, -1.796833398359349410, -6.747090334426651737 ) ) ;
#1540 = AXIS2_PLACEMENT_3D ( 'NONE', #16573, #9359, #6250 ) ;
#1541 = VERTEX_POINT ( 'NONE', #14831 ) ;
#1542 = UNCERTAINTY_MEASURE_WITH_UNIT (LENGTH_MEASURE( 1.000000000000000082E-05 ), #7891, 'distance_accuracy_value', 'NONE');
#1543 = AXIS2_PLACEMENT_3D ( 'NONE', #3701, #15558, #2382 ) ;
#1544 = VECTOR ( 'NONE', #5102, 1000.000000000000000 ) ;
#1545 = VERTEX_POINT ( 'NONE', #11948 ) ;
#1546 = EDGE_CURVE ( 'NONE', #6009, #3698, #17797, .T. ) ;
#1547 = DIRECTION ( 'NONE',  ( -0.9876526153536341335, -0.1566598588826327576, 0.000000000000000000 ) ) ;
#1548 = CARTESIAN_POINT ( 'NONE',  ( -74.19532138785061193, -32.01852751174804013, 8.660254037844417496 ) ) ;
#1549 = DIRECTION ( 'NONE',  ( -0.000000000000000000, -0.000000000000000000, -1.000000000000000000 ) ) ;
#1550 = CARTESIAN_POINT ( 'NONE',  ( -18.39294862037050393, -23.16724548487935564, -17.32050807568878170 ) ) ;
#1551 = FACE_BOUND ( 'NONE', #18483, .T. ) ;
#1553 = EDGE_CURVE ( 'NONE', #16881, #10372, #336, .T. ) ;
#1552 = CYLINDRICAL_SURFACE ( 'NONE', #8140, 1.500000000000001554 ) ;
#1554 = AXIS2_PLACEMENT_3D ( 'NONE', #8106, #14169, #3636 ) ;
#1555 = ADVANCED_FACE ( 'NONE', ( #628 ), #9428, .F. ) ;
#1556 = VERTEX_POINT ( 'NONE', #2126 ) ;
#1557 = ADVANCED_FACE ( 'NONE', ( #12335 ), #2303, .F. ) ;
#1558 = EDGE_CURVE ( 'NONE', #11543, #3425, #11501, .T. ) ;
#1559 = ORIENTED_EDGE ( 'NONE', *, *, #357, .F. ) ;
#1560 = ORIENTED_EDGE ( 'NONE', *, *, #18525, .T. ) ;
#1561 = LINE ( 'NONE', #2786, #13648 ) ;
#1562 = ORIENTED_EDGE ( 'NONE', *, *, #7966, .T. ) ;
#1563 = CARTESIAN_POINT ( 'NONE',  ( -64.60826822105063627, -25.43533591671227612, -4.330127018922180326 ) ) ;
#1564 = LINE ( 'NONE', #7076, #5742 ) ;
#1565 = VERTEX_POINT ( 'NONE', #8196 ) ;
#1566 = AXIS2_PLACEMENT_3D ( 'NONE', #9927, #1151, #9845 ) ;
#1567 = AXIS2_PLACEMENT_3D ( 'NONE', #14048, #1096, #6868 ) ;
#1568 = DIRECTION ( 'NONE',  ( -0.1566598588826321747, 0.9876526153536343555, 0.000000000000000000 ) ) ;
#1569 = DIRECTION ( 'NONE',  ( -0.1566598588826321192, 0.9876526153536342445, 7.798540720466730171E-17 ) ) ;
#1570 = VECTOR ( 'NONE', #2588, 1000.000000000000000 ) ;
#1571 = CARTESIAN_POINT ( 'NONE',  ( -76.90911978745816668, -45.00000000000000711, 20.00000000000002132 ) ) ;
#1572 = ORIENTED_EDGE ( 'NONE', *, *, #15226, .T. ) ;
#1573 = ORIENTED_EDGE ( 'NONE', *, *, #9814, .F. ) ;
#1574 = FACE_BOUND ( 'NONE', #11405, .T. ) ;
#1575 = CARTESIAN_POINT ( 'NONE',  ( -29.21749237908258223, -82.58968536893640078, 7.308518362537324739E-15 ) ) ;
#1576 = EDGE_CURVE ( 'NONE', #16216, #9221, #5161, .T. ) ;
#1577 = AXIS2_PLACEMENT_3D ( 'NONE', #8249, #16791, #3950 ) ;
#1578 = CARTESIAN_POINT ( 'NONE',  ( -11.76885329963143434, -17.05403346649147522, -21.65063509461097979 ) ) ;
#1579 = AXIS2_PLACEMENT_3D ( 'NONE', #972, #5309, #15450 ) ;
#1580 = EDGE_CURVE ( 'NONE', #10670, #15897, #9999, .T. ) ;
#1581 = EDGE_LOOP ( 'NONE', ( #11529, #12659 ) ) ;
#1582 = DIRECTION ( 'NONE',  ( -0.1566598588826321192, 0.9876526153536342445, 7.798540720466731404E-17 ) ) ;
#1583 = AXIS2_PLACEMENT_3D ( 'NONE', #6546, #10874, #3480 ) ;
#1584 = ADVANCED_FACE ( 'NONE', ( #17988 ), #10924, .F. ) ;
#1585 = CIRCLE ( 'NONE', #12135, 1.500000000000000888 ) ;
#1586 = DIRECTION ( 'NONE',  ( 1.000000000000000000, 0.000000000000000000, -3.469446951953612217E-16 ) ) ;
#1587 = CARTESIAN_POINT ( 'NONE',  ( -49.59961335071796640, 39.40051552679455682, -20.00000000000000355 ) ) ;
#1588 = FACE_OUTER_BOUND ( 'NONE', #9304, .T. ) ;
#1589 =( NAMED_UNIT ( * ) PLANE_ANGLE_UNIT ( ) SI_UNIT ( $, .RADIAN. ) );
#1590 = AXIS2_PLACEMENT_3D ( 'NONE', #10536, #7896, #8645 ) ;
#1591 = DIRECTION ( 'NONE',  ( -0.1566598588826321192, 0.9876526153536342445, 7.798540720466730171E-17 ) ) ;
#1592 = CARTESIAN_POINT ( 'NONE',  ( -13.41505053342451426, -80.08312762681433128, 4.330127018922213189 ) ) ;
#1593 = LINE ( 'NONE', #15980, #752 ) ;
#1594 = DIRECTION ( 'NONE',  ( -0.9876526153536341335, -0.1566598588826327021, 0.000000000000000000 ) ) ;
#1595 = VERTEX_POINT ( 'NONE', #12448 ) ;
#1596 = ORIENTED_EDGE ( 'NONE', *, *, #1394, .F. ) ;
#1597 = AXIS2_PLACEMENT_3D ( 'NONE', #17139, #9454, #8021 ) ;
#1598 = CARTESIAN_POINT ( 'NONE',  ( -11.76885329963143434, -17.05403346649147878, -12.99038105676658006 ) ) ;
#1599 = ORIENTED_EDGE ( 'NONE', *, *, #3502, .F. ) ;
#1600 = ORIENTED_EDGE ( 'NONE', *, *, #16700, .T. ) ;
#1601 = VERTEX_POINT ( 'NONE', #6591 ) ;
#1602 = FACE_OUTER_BOUND ( 'NONE', #1914, .T. ) ;
#1603 = ORIENTED_EDGE ( 'NONE', *, *, #17001, .T. ) ;
#1604 = ADVANCED_FACE ( 'NONE', ( #15387 ), #16745, .F. ) ;
#1605 = DIRECTION ( 'NONE',  ( -0.1566598588826321192, 0.9876526153536342445, 7.798540720466731404E-17 ) ) ;
#1606 = DIRECTION ( 'NONE',  ( -0.9876526153536336894, -0.1566598588826349503, 0.000000000000000000 ) ) ;
#1607 = AXIS2_PLACEMENT_3D ( 'NONE', #15466, #12513, #1081 ) ;
#1608 = DIRECTION ( 'NONE',  ( -0.1566598588826321192, 0.9876526153536342445, 7.798540720466731404E-17 ) ) ;
#1609 = EDGE_LOOP ( 'NONE', ( #17915, #16603, #18471, #7883 ) ) ;
#1610 = CARTESIAN_POINT ( 'NONE',  ( -24.31886431249228053, -24.10720463817513703, -12.99038105676658006 ) ) ;
#1611 = CARTESIAN_POINT ( 'NONE',  ( 0.000000000000000000, 0.000000000000000000, -24.99999999999999289 ) ) ;
#1612 = EDGE_CURVE ( 'NONE', #5465, #1095, #15462, .T. ) ;
#1613 = DIRECTION ( 'NONE',  ( -0.1566598588826321747, 0.9876526153536343555, 0.000000000000000000 ) ) ;
#1614 = VERTEX_POINT ( 'NONE', #3435 ) ;
#1615 = LINE ( 'NONE', #17277, #8663 ) ;
#1616 = DIRECTION ( 'NONE',  ( 3.039628882124824168E-17, 0.000000000000000000, -1.000000000000000000 ) ) ;
#1617 = VERTEX_POINT ( 'NONE', #11009 ) ;
#1618 = ORIENTED_EDGE ( 'NONE', *, *, #3328, .F. ) ;
#1619 = CARTESIAN_POINT ( 'NONE',  ( -69.99999999999998579, -45.00000000000000711, -19.99999999999999645 ) ) ;
#1620 = CIRCLE ( 'NONE', #10963, 1.500000000000000888 ) ;
#1621 = VERTEX_POINT ( 'NONE', #18288 ) ;
#1622 = VERTEX_POINT ( 'NONE', #4870 ) ;
#1623 = DIRECTION ( 'NONE',  ( -1.000000000000000000, 0.000000000000000000, 0.000000000000000000 ) ) ;
#1624 = ORIENTED_EDGE ( 'NONE', *, *, #11579, .F. ) ;
#1625 = LINE ( 'NONE', #4721, #2484 ) ;
#1626 = ORIENTED_EDGE ( 'NONE', *, *, #6874, .F. ) ;
#1627 = ADVANCED_FACE ( 'NONE', ( #9323 ), #18078, .F. ) ;
#1628 = ADVANCED_FACE ( 'NONE', ( #16839 ), #9613, .T. ) ;
#1629 = CARTESIAN_POINT ( 'NONE',  ( -77.83221577883584530, 0.3113175352389498385, -4.597871329320426526 ) ) ;
#1630 = ADVANCED_FACE ( 'NONE', ( #18187 ), #2032, .F. ) ;
#1631 = CIRCLE ( 'NONE', #13707, 1.500000000000001332 ) ;
#1632 = LINE ( 'NONE', #7692, #9344 ) ;
#1633 = VERTEX_POINT ( 'NONE', #2220 ) ;
#1634 = FACE_BOUND ( 'NONE', #13474, .T. ) ;
#1635 = ORIENTED_EDGE ( 'NONE', *, *, #118, .T. ) ;
#1636 = CYLINDRICAL_SURFACE ( 'NONE', #3035, 1.500000000000001554 ) ;
#1637 = CARTESIAN_POINT ( 'NONE',  ( -48.80582637539256297, -22.92877817459016399, -8.660254037844380193 ) ) ;
#1638 = CARTESIAN_POINT ( 'NONE',  ( 5.350349158294472218, -77.10659030804430358, 8.660254037844406838 ) ) ;
#1639 = DIRECTION ( 'NONE',  ( -0.9876526153536336894, -0.1566598588826349503, 0.000000000000000000 ) ) ;
#1640 = ORIENTED_EDGE ( 'NONE', *, *, #1083, .F. ) ;
#1641 = VERTEX_POINT ( 'NONE', #721 ) ;
#1642 = ORIENTED_EDGE ( 'NONE', *, *, #1797, .T. ) ;
#1643 = VERTEX_POINT ( 'NONE', #6500 ) ;
#1644 = DIRECTION ( 'NONE',  ( -0.9876526153536336894, -0.1566598588826349503, 0.000000000000000000 ) ) ;
#1645 = ORIENTED_EDGE ( 'NONE', *, *, #17724, .F. ) ;
#1646 = DIRECTION ( 'NONE',  ( -0.3000000000000013767, -0.9539392014169453260, 0.000000000000000000 ) ) ;
#1647 = EDGE_CURVE ( 'NONE', #6106, #13454, #10921, .T. ) ;
#1648 = FACE_OUTER_BOUND ( 'NONE', #12631, .T. ) ;
#1649 = EDGE_CURVE ( 'NONE', #9534, #3195, #13965, .T. ) ;
#1650 = ORIENTED_EDGE ( 'NONE', *, *, #15098, .T. ) ;
#1651 = ORIENTED_EDGE ( 'NONE', *, *, #16533, .T. ) ;
#1652 = ORIENTED_EDGE ( 'NONE', *, *, #6802, .F. ) ;
#1653 = ADVANCED_FACE ( 'NONE', ( #3898 ), #2794, .F. ) ;
#1654 = CARTESIAN_POINT ( 'NONE',  ( -60.16383145195931803, -24.73036655174043119, 1.908195823574487804E-14 ) ) ;
#1655 = CARTESIAN_POINT ( 'NONE',  ( 3.231158466157540765, -19.73726462726228092, -24.99999999999998934 ) ) ;
#1656 = CARTESIAN_POINT ( 'NONE',  ( -77.40662104346073136, 32.93835651487657401, 35.00000000000000000 ) ) ;
#1657 = EDGE_LOOP ( 'NONE', ( #9720, #10349, #3053, #17418 ) ) ;
#1658 = ORIENTED_EDGE ( 'NONE', *, *, #1214, .F. ) ;
#1659 = LINE ( 'NONE', #4766, #11138 ) ;
#1660 = CIRCLE ( 'NONE', #12218, 1.500000000000000444 ) ;
#1661 = CYLINDRICAL_SURFACE ( 'NONE', #8097, 1.500000000000001554 ) ;
#1662 = VERTEX_POINT ( 'NONE', #2592 ) ;
#1663 = DIRECTION ( 'NONE',  ( -0.9876526153536341335, -0.1566598588826327021, 0.000000000000000000 ) ) ;
#1664 = DIRECTION ( 'NONE',  ( -0.1566598588826321192, 0.9876526153536342445, 7.798540720466730171E-17 ) ) ;
#1665 = AXIS2_PLACEMENT_3D ( 'NONE', #9437, #728, #6510 ) ;
#1666 = CARTESIAN_POINT ( 'NONE',  ( -33.20773785067495965, -25.51714336811882688, 17.32050807568881723 ) ) ;
#1667 = EDGE_CURVE ( 'NONE', #7348, #1565, #5734, .T. ) ;
#1668 = EDGE_LOOP ( 'NONE', ( #267, #12837, #12530, #9189 ) ) ;
#1669 = ADVANCED_FACE ( 'NONE', ( #5443, #18376 ), #11388, .F. ) ;
#1670 = CARTESIAN_POINT ( 'NONE',  ( -39.62747985047356281, -26.53543245085592517, -8.660254037844380193 ) ) ;
#1671 = DIRECTION ( 'NONE',  ( -0.9876526153536336894, -0.1566598588826349503, 0.000000000000000000 ) ) ;
#1672 = CYLINDRICAL_SURFACE ( 'NONE', #5958, 1.500000000000000888 ) ;
#1673 = VERTEX_POINT ( 'NONE', #17213 ) ;
#1674 = DIRECTION ( 'NONE',  ( -1.000000000000000000, 0.000000000000000000, 0.000000000000000000 ) ) ;
#1675 = EDGE_CURVE ( 'NONE', #10299, #968, #15489, .T. ) ;
#1677 = EDGE_LOOP ( 'NONE', ( #11273, #1237, #15915, #6184 ) ) ;
#1676 = CARTESIAN_POINT ( 'NONE',  ( -88.82622559915370175, -29.27674910825304977, 25.00000000000001776 ) ) ;
#1678 = ORIENTED_EDGE ( 'NONE', *, *, #11185, .T. ) ;
#1679 = AXIS2_PLACEMENT_3D ( 'NONE', #1950, #4958, #16653 ) ;
#1680 = VERTEX_POINT ( 'NONE', #2865 ) ;
#1681 = CARTESIAN_POINT ( 'NONE',  ( 73.09088021254186174, 1.387778780781445676E-14, -2.500000000000000444 ) ) ;
#1682 = VERTEX_POINT ( 'NONE', #9803 ) ;
#1683 = DIRECTION ( 'NONE',  ( 0.000000000000000000, 1.000000000000000000, -1.224646799147353207E-16 ) ) ;
#1684 = DIRECTION ( 'NONE',  ( 2.735665993912342121E-16, 0.000000000000000000, 1.000000000000000000 ) ) ;
#1685 = ORIENTED_EDGE ( 'NONE', *, *, #10006, .F. ) ;
#1686 = CARTESIAN_POINT ( 'NONE',  ( -56.37793930130741415, -86.89783148820879433, -4.330127018922185655 ) ) ;
#1687 = SURFACE_STYLE_USAGE ( .BOTH. , #11800 ) ;
#1688 = DIRECTION ( 'NONE',  ( 0.000000000000000000, 0.000000000000000000, 1.000000000000000000 ) ) ;
#1689 = CIRCLE ( 'NONE', #12259, 1.500000000000000444 ) ;
#1690 = FACE_OUTER_BOUND ( 'NONE', #15751, .T. ) ;
#1691 = FACE_BOUND ( 'NONE', #4055, .T. ) ;
#1692 = CARTESIAN_POINT ( 'NONE',  ( -57.89905323451571206, -29.43363984018462176, -17.32050807568878170 ) ) ;
#1693 = FACE_OUTER_BOUND ( 'NONE', #13800, .T. ) ;
#1694 = EDGE_CURVE ( 'NONE', #7684, #18620, #1198, .T. ) ;
#1695 = CARTESIAN_POINT ( 'NONE',  ( -46.33669483700847280, -22.53712852738359373, 12.99038105676661736 ) ) ;
#1697 = ORIENTED_EDGE ( 'NONE', *, *, #12586, .T. ) ;
#1696 = LINE ( 'NONE', #14860, #7256 ) ;
#1698 = ORIENTED_EDGE ( 'NONE', *, *, #5305, .F. ) ;
#1699 = CARTESIAN_POINT ( 'NONE',  ( -61.31620237807555895, -87.68113078262196325, 21.65063509461101532 ) ) ;
#1700 = AXIS2_PLACEMENT_3D ( 'NONE', #9194, #15557, #11282 ) ;
#1701 = ORIENTED_EDGE ( 'NONE', *, *, #4888, .T. ) ;
#1702 = EDGE_CURVE ( 'NONE', #18222, #2420, #15775, .T. ) ;
#1703 = VERTEX_POINT ( 'NONE', #12904 ) ;
#1704 = DIRECTION ( 'NONE',  ( -0.1566598588826321747, 0.9876526153536343555, 0.000000000000000000 ) ) ;
#1705 = ORIENTED_EDGE ( 'NONE', *, *, #3696, .F. ) ;
#1706 = AXIS2_PLACEMENT_3D ( 'NONE', #9851, #15620, #2647 ) ;
#1707 = DIRECTION ( 'NONE',  ( -0.000000000000000000, -0.000000000000000000, 1.000000000000000000 ) ) ;
#1708 = CYLINDRICAL_SURFACE ( 'NONE', #2816, 1.500000000000001554 ) ;
#1709 = ORIENTED_EDGE ( 'NONE', *, *, #10798, .T. ) ;
#1710 = DIRECTION ( 'NONE',  ( -0.1566598588826321192, 0.9876526153536342445, 7.798540720466731404E-17 ) ) ;
#1711 = ORIENTED_EDGE ( 'NONE', *, *, #6359, .T. ) ;
#1712 = LINE ( 'NONE', #16310, #5525 ) ;
#1713 = ORIENTED_EDGE ( 'NONE', *, *, #7104, .T. ) ;
#1714 = EDGE_CURVE ( 'NONE', #7134, #8567, #1464, .T. ) ;
#1715 = DIRECTION ( 'NONE',  ( -0.1566598588826321747, 0.9876526153536343555, 0.000000000000000000 ) ) ;
#1716 = CARTESIAN_POINT ( 'NONE',  ( -66.08974714408108753, -25.67032570503621969, -4.330127018922180326 ) ) ;
#1717 = ORIENTED_EDGE ( 'NONE', *, *, #11760, .T. ) ;
#1718 = ADVANCED_FACE ( 'NONE', ( #17513 ), #12778, .F. ) ;
#1719 = ORIENTED_EDGE ( 'NONE', *, *, #16557, .T. ) ;
#1720 = ORIENTED_EDGE ( 'NONE', *, *, #1770, .F. ) ;
#1721 = CYLINDRICAL_SURFACE ( 'NONE', #18708, 1.500000000000001554 ) ;
#1722 = VECTOR ( 'NONE', #14742, 1000.000000000000000 ) ;
#1723 = AXIS2_PLACEMENT_3D ( 'NONE', #1795, #567, #17457 ) ;
#1724 = FACE_BOUND ( 'NONE', #13194, .T. ) ;
#1725 = DIRECTION ( 'NONE',  ( 0.000000000000000000, 0.000000000000000000, 1.000000000000000000 ) ) ;
#1726 = CARTESIAN_POINT ( 'NONE',  ( -129.1404785418517918, -2.850701963179328668, 9.951701414186818625E-16 ) ) ;
#1727 = VECTOR ( 'NONE', #15326, 1000.000000000000000 ) ;
#1728 = ORIENTED_EDGE ( 'NONE', *, *, #16724, .T. ) ;
#1729 = DIRECTION ( 'NONE',  ( -0.1566598588826321747, 0.9876526153536343555, 0.000000000000000000 ) ) ;
#1730 = CIRCLE ( 'NONE', #12309, 1.500000000000000000 ) ;
#1731 = DIRECTION ( 'NONE',  ( -0.1566598588826321192, 0.9876526153536342445, 7.798540720466731404E-17 ) ) ;
#1732 = DIRECTION ( 'NONE',  ( -0.000000000000000000, -0.000000000000000000, 1.000000000000000000 ) ) ;
#1733 = EDGE_CURVE ( 'NONE', #18389, #16485, #12664, .T. ) ;
#1734 = CARTESIAN_POINT ( 'NONE',  ( -70.46959788260221558, 45.19981602042874869, -5.279908564046689179 ) ) ;
#1735 = EDGE_CURVE ( 'NONE', #13724, #6259, #17627, .T. ) ;
#1736 = DIRECTION ( 'NONE',  ( 0.000000000000000000, 0.000000000000000000, 1.000000000000000000 ) ) ;
#1737 = ORIENTED_EDGE ( 'NONE', *, *, #17505, .F. ) ;
#1738 = ORIENTED_EDGE ( 'NONE', *, *, #10215, .F. ) ;
#1739 = DIRECTION ( 'NONE',  ( -0.1566598588826321192, 0.9876526153536342445, 7.798540720466730171E-17 ) ) ;
#1740 = EDGE_CURVE ( 'NONE', #6097, #10127, #1277, .T. ) ;
#1741 = LINE ( 'NONE', #13570, #3025 ) ;
#1742 = AXIS2_PLACEMENT_3D ( 'NONE', #9521, #17990, #9616 ) ;
#1743 = ORIENTED_EDGE ( 'NONE', *, *, #15544, .F. ) ;
#1744 = LINE ( 'NONE', #5844, #5974 ) ;
#1745 = AXIS2_PLACEMENT_3D ( 'NONE', #12041, #16351, #3340 ) ;
#1746 = CARTESIAN_POINT ( 'NONE',  ( -58.68235252892886678, -24.49537676341648051, -8.660254037844380193 ) ) ;
#1747 = ORIENTED_EDGE ( 'NONE', *, *, #13227, .T. ) ;
#1748 = ORIENTED_EDGE ( 'NONE', *, *, #1904, .T. ) ;
#1749 = CARTESIAN_POINT ( 'NONE',  ( 3.868870235264020963, -77.34158009636824715, -17.32050807568878525 ) ) ;
#1750 = FACE_BOUND ( 'NONE', #7647, .T. ) ;
#1751 = CARTESIAN_POINT ( 'NONE',  ( 0.000000000000000000, 0.000000000000000000, 24.99999999999999289 ) ) ;
#1752 = AXIS2_PLACEMENT_3D ( 'NONE', #11601, #69, #14559 ) ;
#1753 = DIRECTION ( 'NONE',  ( -0.1566598588826321192, 0.9876526153536342445, 7.798540720466731404E-17 ) ) ;
#1754 = CIRCLE ( 'NONE', #546, 1.500000000000000888 ) ;
#1755 = EDGE_LOOP ( 'NONE', ( #2947, #4083 ) ) ;
#1756 = LINE ( 'NONE', #17246, #3586 ) ;
#1757 = DIRECTION ( 'NONE',  ( -0.1566598588826321192, 0.9876526153536342445, 7.798540720466731404E-17 ) ) ;
#1758 = DIRECTION ( 'NONE',  ( 0.000000000000000000, 0.000000000000000000, 1.000000000000000000 ) ) ;
#1759 = EDGE_CURVE ( 'NONE', #10340, #4741, #6710, .T. ) ;
#1760 = CYLINDRICAL_SURFACE ( 'NONE', #16250, 1.500000000000000888 ) ;
#1761 = EDGE_LOOP ( 'NONE', ( #6420, #11707, #14054, #2020 ) ) ;
#1762 = DIRECTION ( 'NONE',  ( 1.000000000000000000, 0.000000000000000000, 0.000000000000000000 ) ) ;
#1763 = ORIENTED_EDGE ( 'NONE', *, *, #14939, .T. ) ;
#1764 = AXIS2_PLACEMENT_3D ( 'NONE', #13358, #17755, #4728 ) ;
#1765 = AXIS2_PLACEMENT_3D ( 'NONE', #9732, #14062, #18386 ) ;
#1766 = ORIENTED_EDGE ( 'NONE', *, *, #6857, .F. ) ;
#1767 = EDGE_CURVE ( 'NONE', #11126, #13246, #17317, .T. ) ;
#1768 = AXIS2_PLACEMENT_3D ( 'NONE', #17362, #4347, #18627 ) ;
#1769 = EDGE_LOOP ( 'NONE', ( #14744, #11820 ) ) ;
#1770 = EDGE_CURVE ( 'NONE', #11020, #1828, #4868, .T. ) ;
#1771 = CARTESIAN_POINT ( 'NONE',  ( -3.382878129548352319, -13.70423786865302773, 19.99999999999999645 ) ) ;
#1772 = AXIS2_PLACEMENT_3D ( 'NONE', #111, #4368, #14237 ) ;
#1773 = CARTESIAN_POINT ( 'NONE',  ( -81.73462711737164454, 33.01666666666666572, -30.00000000000000000 ) ) ;
#1774 = DIRECTION ( 'NONE',  ( -0.1566598588826321192, 0.9876526153536342445, 7.798540720466730171E-17 ) ) ;
#1775 = CIRCLE ( 'NONE', #12351, 1.499999999999999556 ) ;
#1776 = ORIENTED_EDGE ( 'NONE', *, *, #5784, .F. ) ;
#1777 = DIRECTION ( 'NONE',  ( -0.1566598588826321192, 0.9876526153536342445, 7.798540720466730171E-17 ) ) ;
#1778 = DIRECTION ( 'NONE',  ( -0.1566598588826321192, 0.9876526153536342445, 7.798540720466730171E-17 ) ) ;
#1779 = EDGE_LOOP ( 'NONE', ( #5664, #8692, #1990, #11428 ) ) ;
#1780 = VECTOR ( 'NONE', #11064, 1000.000000000000114 ) ;
#1781 = DIRECTION ( 'NONE',  ( 0.000000000000000000, 0.000000000000000000, 1.000000000000000000 ) ) ;
#1782 = CIRCLE ( 'NONE', #9962, 1.500000000000000444 ) ;
#1783 = CARTESIAN_POINT ( 'NONE',  ( 0.000000000000000000, 0.000000000000000000, 30.00000000000000000 ) ) ;
#1784 = CARTESIAN_POINT ( 'NONE',  ( -30.04042668367358360, -19.95224085582016471, -12.99038105676658006 ) ) ;
#1785 = VERTEX_POINT ( 'NONE', #5591 ) ;
#1787 = EDGE_LOOP ( 'NONE', ( #7734, #9700, #6659, #13001 ) ) ;
#1786 = CARTESIAN_POINT ( 'NONE',  ( -4.565812005419673802, -20.97400746052251108, -4.330127018922184767 ) ) ;
#1788 = VECTOR ( 'NONE', #8869, 1000.000000000000000 ) ;
#1789 = EDGE_LOOP ( 'NONE', ( #18449, #5393, #112, #10399 ) ) ;
#1790 = DIRECTION ( 'NONE',  ( -0.1566598588826321747, 0.9876526153536343555, 0.000000000000000000 ) ) ;
#1791 = AXIS2_PLACEMENT_3D ( 'NONE', #17285, #2759, #5605 ) ;
#1792 = VERTEX_POINT ( 'NONE', #15900 ) ;
#1793 = ADVANCED_FACE ( 'NONE', ( #4423 ), #6927, .F. ) ;
#1794 = ORIENTED_EDGE ( 'NONE', *, *, #18353, .F. ) ;
#1795 = CARTESIAN_POINT ( 'NONE',  ( -30.73860631229088369, -25.12549372091224598, 4.330127018922217630 ) ) ;
#1796 = AXIS2_PLACEMENT_3D ( 'NONE', #14290, #6726, #1321 ) ;
#1797 = EDGE_CURVE ( 'NONE', #8732, #9690, #4574, .T. ) ;
#1798 = AXIS2_PLACEMENT_3D ( 'NONE', #3437, #9328, #11950 ) ;
#1799 = AXIS2_PLACEMENT_3D ( 'NONE', #5863, #17431, #4418 ) ;
#1800 = VECTOR ( 'NONE', #10558, 1000.000000000000000 ) ;
#1801 = CYLINDRICAL_SURFACE ( 'NONE', #9760, 145.0000000000000284 ) ;
#1802 = VERTEX_POINT ( 'NONE', #10203 ) ;
#1803 = ADVANCED_FACE ( 'NONE', ( #11255 ), #10027, .F. ) ;
#1804 = DIRECTION ( 'NONE',  ( -0.1566598588826321192, 0.9876526153536342445, 7.798540720466730171E-17 ) ) ;
#1805 = AXIS2_PLACEMENT_3D ( 'NONE', #11229, #7005, #3925 ) ;
#1806 = CARTESIAN_POINT ( 'NONE',  ( -67.77557938805200877, -31.00023842901093118, 8.660254037844417496 ) ) ;
#1807 = AXIS2_PLACEMENT_3D ( 'NONE', #2496, #8280, #6401 ) ;
#1808 = CARTESIAN_POINT ( 'NONE',  ( -33.16810284049710589, -83.21632480446695013, -4.330127018922185655 ) ) ;
#1809 = DIRECTION ( 'NONE',  ( -0.1566598588826321192, 0.9876526153536342445, 7.798540720466731404E-17 ) ) ;
#1810 = ORIENTED_EDGE ( 'NONE', *, *, #14128, .F. ) ;
#1811 = AXIS2_PLACEMENT_3D ( 'NONE', #12247, #17905, #18082 ) ;
#1812 = FACE_OUTER_BOUND ( 'NONE', #16311, .T. ) ;
#1813 = ORIENTED_EDGE ( 'NONE', *, *, #12144, .T. ) ;
#1814 = LINE ( 'NONE', #7603, #7719 ) ;
#1815 = AXIS2_PLACEMENT_3D ( 'NONE', #10512, #26, #15927 ) ;
#1816 = DIRECTION ( 'NONE',  ( -0.1566598588826321192, 0.9876526153536342445, 7.798540720466730171E-17 ) ) ;
#1817 = EDGE_LOOP ( 'NONE', ( #2784, #14936 ) ) ;
#1818 = ORIENTED_EDGE ( 'NONE', *, *, #4013, .F. ) ;
#1819 = CIRCLE ( 'NONE', #12400, 1.500000000000000888 ) ;
#1820 = VERTEX_POINT ( 'NONE', #17267 ) ;
#1821 = DIRECTION ( 'NONE',  ( 0.000000000000000000, 0.000000000000000000, 1.000000000000000000 ) ) ;
#1822 = AXIS2_PLACEMENT_3D ( 'NONE', #6529, #8834, #10757 ) ;
#1823 = FACE_BOUND ( 'NONE', #3030, .T. ) ;
#1824 = AXIS2_PLACEMENT_3D ( 'NONE', #6485, #16513, #17879 ) ;
#1825 = VERTEX_POINT ( 'NONE', #11527 ) ;
#1826 = EDGE_CURVE ( 'NONE', #11513, #15461, #965, .T. ) ;
#1827 = CIRCLE ( 'NONE', #14256, 18.88854657239857815 ) ;
#1828 = VERTEX_POINT ( 'NONE', #15612 ) ;
#1829 = VERTEX_POINT ( 'NONE', #2904 ) ;
#1830 = EDGE_CURVE ( 'NONE', #6534, #3287, #14280, .T. ) ;
#1831 = AXIS2_PLACEMENT_3D ( 'NONE', #13760, #10655, #16642 ) ;
#1832 = DIRECTION ( 'NONE',  ( -0.1566598588826321192, 0.9876526153536342445, 7.798540720466731404E-17 ) ) ;
#1833 = ORIENTED_EDGE ( 'NONE', *, *, #7332, .T. ) ;
#1834 = DIRECTION ( 'NONE',  ( 0.000000000000000000, 0.000000000000000000, 1.000000000000000000 ) ) ;
#1836 = DIRECTION ( 'NONE',  ( -0.000000000000000000, -0.000000000000000000, -1.000000000000000000 ) ) ;
#1835 = AXIS2_PLACEMENT_3D ( 'NONE', #9916, #7459, #4331 ) ;
#1837 = DIRECTION ( 'NONE',  ( -0.9876526153536336894, -0.1566598588826349503, 0.000000000000000000 ) ) ;
#1838 = DIRECTION ( 'NONE',  ( -0.1566598588826321192, 0.9876526153536342445, 7.798540720466730171E-17 ) ) ;
#1839 = VERTEX_POINT ( 'NONE', #14204 ) ;
#1840 = ORIENTED_EDGE ( 'NONE', *, *, #10688, .T. ) ;
#1841 = CARTESIAN_POINT ( 'NONE',  ( -13.45468554360235203, -22.38394619046619383, 1.869203119972154228E-14 ) ) ;
#1842 = AXIS2_PLACEMENT_3D ( 'NONE', #13120, #18687, #8872 ) ;
#1843 = LINE ( 'NONE', #7633, #14151 ) ;
#1844 = VECTOR ( 'NONE', #14175, 1000.000000000000000 ) ;
#1845 = ORIENTED_EDGE ( 'NONE', *, *, #13785, .F. ) ;
#1846 = FACE_OUTER_BOUND ( 'NONE', #15073, .T. ) ;
#1847 = AXIS2_PLACEMENT_3D ( 'NONE', #9884, #1378, #5635 ) ;
#1848 = LINE ( 'NONE', #7639, #2697 ) ;
#1849 = VECTOR ( 'NONE', #16760, 1000.000000000000000 ) ;
#1850 = EDGE_CURVE ( 'NONE', #5249, #13731, #8819, .T. ) ;
#1851 = CARTESIAN_POINT ( 'NONE',  ( -48.97054468615519340, -85.72288254658904805, -17.32050807568878525 ) ) ;
#1852 = EDGE_CURVE ( 'NONE', #5489, #2351, #11341, .T. ) ;
#1853 = CARTESIAN_POINT ( 'NONE',  ( -51.47931123471710890, -28.41535075744750571, 1.887572821959364500E-14 ) ) ;
#1854 = ADVANCED_FACE ( 'NONE', ( #7211 ), #14942, .F. ) ;
#1855 = AXIS2_PLACEMENT_3D ( 'NONE', #430, #3432, #1939 ) ;
#1856 = DIRECTION ( 'NONE',  ( 0.000000000000000000, 0.000000000000000000, 1.000000000000000000 ) ) ;
#1857 = SURFACE_SIDE_STYLE ('',( #13401 ) ) ;
#1858 = AXIS2_PLACEMENT_3D ( 'NONE', #2831, #12863, #17157 ) ;
#1859 = AXIS2_PLACEMENT_3D ( 'NONE', #13139, #3097, #17645 ) ;
#1860 = FACE_OUTER_BOUND ( 'NONE', #5789, .T. ) ;
#1861 = ORIENTED_EDGE ( 'NONE', *, *, #10638, .T. ) ;
#1862 = ORIENTED_EDGE ( 'NONE', *, *, #4493, .T. ) ;
#1863 = DIRECTION ( 'NONE',  ( 0.000000000000000000, 0.000000000000000000, 1.000000000000000000 ) ) ;
#1864 = VERTEX_POINT ( 'NONE', #16382 ) ;
#1865 = CIRCLE ( 'NONE', #17945, 1.500000000000001332 ) ;
#1866 = ORIENTED_EDGE ( 'NONE', *, *, #2081, .T. ) ;
#1867 = AXIS2_PLACEMENT_3D ( 'NONE', #13080, #18549, #14231 ) ;
#1868 = ADVANCED_BREP_SHAPE_REPRESENTATION ( '', ( #2591, #18772 ), #7243 ) ;
#1869 = CARTESIAN_POINT ( 'NONE',  ( -43.04462899403339549, -84.78292339329327376, 12.99038105676661203 ) ) ;
#1870 = AXIS2_PLACEMENT_3D ( 'NONE', #8436, #15346, #2468 ) ;
#1871 = EDGE_CURVE ( 'NONE', #2581, #18009, #5498, .T. ) ;
#1872 = LINE ( 'NONE', #13414, #7030 ) ;
#1873 = CARTESIAN_POINT ( 'NONE',  ( -129.1404785418517918, 8.649298036820674440, -5.500000000000000000 ) ) ;
#1874 = DIRECTION ( 'NONE',  ( -0.1566598588826321192, 0.9876526153536342445, 7.798540720466730171E-17 ) ) ;
#1875 = DIRECTION ( 'NONE',  ( 1.000000000000000000, 0.000000000000000000, 0.000000000000000000 ) ) ;
#1876 = ORIENTED_EDGE ( 'NONE', *, *, #18633, .T. ) ;
#1877 = EDGE_CURVE ( 'NONE', #10500, #12364, #7467, .T. ) ;
#1878 = AXIS2_PLACEMENT_3D ( 'NONE', #12178, #13333, #10751 ) ;
#1879 = CARTESIAN_POINT ( 'NONE',  ( -0.9046745307415022808, -15.33077501878252136, -8.660254037844383745 ) ) ;
#1880 = EDGE_LOOP ( 'NONE', ( #10584, #12657 ) ) ;
#1881 = LINE ( 'NONE', #3373, #15321 ) ;
#1882 = EDGE_CURVE ( 'NONE', #5969, #7962, #258, .T. ) ;
#1883 = ORIENTED_EDGE ( 'NONE', *, *, #14085, .T. ) ;
#1885 = EDGE_LOOP ( 'NONE', ( #13407, #2564 ) ) ;
#1884 = FACE_OUTER_BOUND ( 'NONE', #16108, .T. ) ;
#1886 = AXIS2_PLACEMENT_3D ( 'NONE', #4481, #1832, #319 ) ;
#1887 = DIRECTION ( 'NONE',  ( -0.9876526153536336894, -0.1566598588826349503, 0.000000000000000000 ) ) ;
#1888 = ORIENTED_EDGE ( 'NONE', *, *, #5404, .F. ) ;
#1889 = ORIENTED_EDGE ( 'NONE', *, *, #5855, .T. ) ;
#1890 = ORIENTED_EDGE ( 'NONE', *, *, #17831, .T. ) ;
#1891 = CARTESIAN_POINT ( 'NONE',  ( -62.13913668266654611, -25.04368626950570587, 17.32050807568881723 ) ) ;
#1892 = AXIS2_PLACEMENT_3D ( 'NONE', #2101, #16612, #9020 ) ;
#1893 = AXIS2_PLACEMENT_3D ( 'NONE', #1190, #7154, #2949 ) ;
#1894 = DIRECTION ( 'NONE',  ( -1.000000000000000000, -1.224646799147353207E-16, 0.000000000000000000 ) ) ;
#1895 = ORIENTED_EDGE ( 'NONE', *, *, #5420, .F. ) ;
#1896 = DIRECTION ( 'NONE',  ( -0.1566598588826321192, 0.9876526153536342445, 7.798540720466730171E-17 ) ) ;
#1897 = DIRECTION ( 'NONE',  ( -0.9876526153536336894, -0.1566598588826349503, 0.000000000000000000 ) ) ;
#1898 = CARTESIAN_POINT ( 'NONE',  ( -39.13365354279672914, -26.45710252141460828, 4.330127018922217630 ) ) ;
#1899 = UNCERTAINTY_MEASURE_WITH_UNIT (LENGTH_MEASURE( 1.000000000000000082E-05 ), #7601, 'distance_accuracy_value', 'NONE');
#1900 = DIRECTION ( 'NONE',  ( 1.000000000000000000, 0.000000000000000000, 0.000000000000000000 ) ) ;
#1901 = CYLINDRICAL_SURFACE ( 'NONE', #12698, 1.500000000000001554 ) ;
#1902 = CARTESIAN_POINT ( 'NONE',  ( -53.74408945216072198, -23.71207746900331870, -17.32050807568878170 ) ) ;
#1903 = VERTEX_POINT ( 'NONE', #8794 ) ;
#1904 = EDGE_CURVE ( 'NONE', #13791, #16138, #6237, .T. ) ;
#1905 = EDGE_CURVE ( 'NONE', #1188, #9148, #9739, .T. ) ;
#1906 = VERTEX_POINT ( 'NONE', #3176 ) ;
#1907 = CIRCLE ( 'NONE', #5556, 1.499999999999999556 ) ;
#1908 = CYLINDRICAL_SURFACE ( 'NONE', #9225, 1.500000000000001554 ) ;
#1909 = DIRECTION ( 'NONE',  ( -0.1566598588826321747, 0.9876526153536343555, 0.000000000000000000 ) ) ;
#1910 = ADVANCED_FACE ( 'NONE', ( #6051 ), #16187, .F. ) ;
#1911 = ORIENTED_EDGE ( 'NONE', *, *, #24, .F. ) ;
#1912 = ORIENTED_EDGE ( 'NONE', *, *, #2458, .F. ) ;
#1913 = EDGE_LOOP ( 'NONE', ( #17983, #10408, #13405, #10472 ) ) ;
#1914 = EDGE_LOOP ( 'NONE', ( #17770, #12813, #13909, #3661 ) ) ;
#1915 = EDGE_LOOP ( 'NONE', ( #4337, #8057 ) ) ;
#1916 = CARTESIAN_POINT ( 'NONE',  ( 5.481473465377021625, 12.88229205725314763, -19.99999999999998934 ) ) ;
#1917 = ORIENTED_EDGE ( 'NONE', *, *, #4374, .T. ) ;
#1918 = FACE_BOUND ( 'NONE', #15833, .T. ) ;
#1919 = ORIENTED_EDGE ( 'NONE', *, *, #6145, .T. ) ;
#1920 = AXIS2_PLACEMENT_3D ( 'NONE', #6240, #11702, #15031 ) ;
#1921 = ORIENTED_EDGE ( 'NONE', *, *, #9782, .T. ) ;
#1922 = ORIENTED_EDGE ( 'NONE', *, *, #526, .T. ) ;
#1923 = DIRECTION ( 'NONE',  ( 0.9201637183752249260, -0.3915338189555017667, 0.000000000000000000 ) ) ;
#1924 = CYLINDRICAL_SURFACE ( 'NONE', #7581, 1.500000000000001554 ) ;
#1925 = DIRECTION ( 'NONE',  ( 1.000000000000000000, 0.000000000000000000, 0.000000000000000000 ) ) ;
#1926 = CARTESIAN_POINT ( 'NONE',  ( -16.70711637639958269, -17.83733276090463704, -12.99038105676658006 ) ) ;
#1927 = DIRECTION ( 'NONE',  ( 8.693966348389027220E-17, -1.991237296706374949E-16, 1.000000000000000000 ) ) ;
#1928 = CARTESIAN_POINT ( 'NONE',  ( -38.14600092744309734, -26.30044266253198160, -8.660254037844380193 ) ) ;
#1929 = ORIENTED_EDGE ( 'NONE', *, *, #17709, .T. ) ;
#1930 = EDGE_LOOP ( 'NONE', ( #9001, #9036, #2188, #4675 ) ) ;
#1931 = AXIS2_PLACEMENT_3D ( 'NONE', #12368, #2330, #1224 ) ;
#1932 = CARTESIAN_POINT ( 'NONE',  ( 3.231158466157545206, -19.73726462726228092, 30.00000000000000000 ) ) ;
#1933 = EDGE_CURVE ( 'NONE', #6009, #10091, #5194, .T. ) ;
#1934 = CARTESIAN_POINT ( 'NONE',  ( -49.26481467677530190, 51.83848025225071865, -20.00000000000001421 ) ) ;
#1935 = FACE_OUTER_BOUND ( 'NONE', #11244, .T. ) ;
#1936 = DIRECTION ( 'NONE',  ( -0.000000000000000000, -0.000000000000000000, -1.000000000000000000 ) ) ;
#1937 = ORIENTED_EDGE ( 'NONE', *, *, #18207, .T. ) ;
#1938 = VERTEX_POINT ( 'NONE', #13231 ) ;
#1939 = DIRECTION ( 'NONE',  ( 0.000000000000000000, -1.000000000000000000, -1.203364738757079611E-16 ) ) ;
#1940 = EDGE_CURVE ( 'NONE', #10290, #15025, #1872, .T. ) ;
#1941 = DIRECTION ( 'NONE',  ( -0.1566598588826321192, 0.9876526153536342445, 7.798540720466731404E-17 ) ) ;
#1942 = CARTESIAN_POINT ( 'NONE',  ( 55.85952145814821534, 6.938893903907228378E-15, -2.500000000000000000 ) ) ;
#1943 = CARTESIAN_POINT ( 'NONE',  ( -90.00000000000000000, 34.99999999999999289, 35.00000000000000000 ) ) ;
#1944 = PRESENTATION_STYLE_ASSIGNMENT (( #8874 ) ) ;
#1945 = ORIENTED_EDGE ( 'NONE', *, *, #13940, .T. ) ;
#1946 = DIRECTION ( 'NONE',  ( -0.1566598588826321747, 0.9876526153536343555, 0.000000000000000000 ) ) ;
#1947 = EDGE_CURVE ( 'NONE', #15938, #1312, #8966, .T. ) ;
#1948 = DIRECTION ( 'NONE',  ( -0.1566598588826321747, 0.9876526153536343555, 0.000000000000000000 ) ) ;
#1949 = ORIENTED_EDGE ( 'NONE', *, *, #11524, .F. ) ;
#1950 = CARTESIAN_POINT ( 'NONE',  ( -76.90911978745816668, -45.00000000000000711, 20.00000000000002132 ) ) ;
#1951 = ORIENTED_EDGE ( 'NONE', *, *, #16965, .T. ) ;
#1952 = ORIENTED_EDGE ( 'NONE', *, *, #8811, .F. ) ;
#1953 = DIRECTION ( 'NONE',  ( -0.9876526153536336894, -0.1566598588826350336, 0.000000000000000000 ) ) ;
#1954 = ADVANCED_FACE ( 'NONE', ( #11701 ), #4892, .F. ) ;
#1955 = ORIENTED_EDGE ( 'NONE', *, *, #1830, .T. ) ;
#1956 = EDGE_CURVE ( 'NONE', #15309, #12162, #10303, .T. ) ;
#1957 = ORIENTED_EDGE ( 'NONE', *, *, #1394, .T. ) ;
#1958 = EDGE_CURVE ( 'NONE', #7789, #2452, #7620, .T. ) ;
#1959 = CARTESIAN_POINT ( 'NONE',  ( -34.97868976044173195, -20.73554015023333008, 4.330127018922218518 ) ) ;
#1960 = DIRECTION ( 'NONE',  ( -0.1566598588826321192, 0.9876526153536342445, 7.798540720466730171E-17 ) ) ;
#1961 = CARTESIAN_POINT ( 'NONE',  ( -89.99999999999998579, -35.00000000000001421, 30.00000000000005329 ) ) ;
#1962 = CYLINDRICAL_SURFACE ( 'NONE', #4186, 2.500000000000002220 ) ;
#1963 = CARTESIAN_POINT ( 'NONE',  ( -36.62488699423481364, -83.76463431055616127, -4.330127018922185655 ) ) ;
#1964 = PRODUCT_DEFINITION_SHAPE ( 'NONE', 'NONE',  #1533 ) ;
#1965 = CARTESIAN_POINT ( 'NONE',  ( -90.00000000000000000, 34.99999999999999289, 35.00000000000000000 ) ) ;
#1966 = CARTESIAN_POINT ( 'NONE',  ( -41.60278508118079799, -26.84875216862118918, 1.887572821959364500E-14 ) ) ;
#1967 = ORIENTED_EDGE ( 'NONE', *, *, #14405, .T. ) ;
#1968 = DIRECTION ( 'NONE',  ( -0.1566598588826321747, 0.9876526153536343555, 0.000000000000000000 ) ) ;
#1969 = CIRCLE ( 'NONE', #5310, 1.500000000000000888 ) ;
#1970 = EDGE_CURVE ( 'NONE', #12438, #15242, #8533, .T. ) ;
#1972 = EDGE_LOOP ( 'NONE', ( #15195, #7068 ) ) ;
#1971 = CARTESIAN_POINT ( 'NONE',  ( -38.14600092744310444, -26.30044266253198160, 8.660254037844417496 ) ) ;
#1973 = ADVANCED_FACE ( 'NONE', ( #10477 ), #4521, .F. ) ;
#1974 = DIRECTION ( 'NONE',  ( -0.9876526153536341335, -0.1566598588826327021, 0.000000000000000000 ) ) ;
#1975 = EDGE_CURVE ( 'NONE', #10686, #18371, #915, .T. ) ;
#1976 = ORIENTED_EDGE ( 'NONE', *, *, #16677, .F. ) ;
#1977 = EDGE_LOOP ( 'NONE', ( #11451, #14276, #11198, #4345 ) ) ;
#1978 = DIRECTION ( 'NONE',  ( 1.000000000000000000, 0.000000000000000000, 0.000000000000000000 ) ) ;
#1979 = CARTESIAN_POINT ( 'NONE',  ( -10.98555400521827607, -21.99229654325962002, 12.99038105676661381 ) ) ;
#1980 = ORIENTED_EDGE ( 'NONE', *, *, #10414, .F. ) ;
#1981 = CARTESIAN_POINT ( 'NONE',  ( -41.60278508118080509, -26.84875216862118918, -17.32050807568878170 ) ) ;
#1982 = CIRCLE ( 'NONE', #9551, 1.499999999999999556 ) ;
#1983 = ORIENTED_EDGE ( 'NONE', *, *, #2995, .F. ) ;
#1984 = CARTESIAN_POINT ( 'NONE',  ( -0.5755665338273054932, -78.04654946134009208, 4.330127018922209636 ) ) ;
#1985 = CARTESIAN_POINT ( 'NONE',  ( 0.000000000000000000, 0.000000000000000000, 30.00000000000000000 ) ) ;
#1986 = LINE ( 'NONE', #7772, #2958 ) ;
#1987 = CARTESIAN_POINT ( 'NONE',  ( -31.52190560670403841, -20.18723064414411184, -4.330127018922180326 ) ) ;
#1988 = DIRECTION ( 'NONE',  ( -1.000000000000000000, 0.000000000000000000, 0.000000000000000000 ) ) ;
#1989 = CARTESIAN_POINT ( 'NONE',  ( -31.52190560670403841, -20.18723064414412249, 21.65063509461102242 ) ) ;
#1990 = ORIENTED_EDGE ( 'NONE', *, *, #3378, .T. ) ;
#1991 = FACE_BOUND ( 'NONE', #11735, .T. ) ;
#1992 = DIRECTION ( 'NONE',  ( -0.1566598588826321192, 0.9876526153536342445, 7.798540720466731404E-17 ) ) ;
#1993 = VERTEX_POINT ( 'NONE', #6984 ) ;
#1994 = CIRCLE ( 'NONE', #13775, 150.0000000000000000 ) ;
#1995 = CARTESIAN_POINT ( 'NONE',  ( 73.09088021254186174, 1.387778780781445676E-14, 19.99999999999997513 ) ) ;
#1996 = FACE_OUTER_BOUND ( 'NONE', #18432, .T. ) ;
#1997 = AXIS2_PLACEMENT_3D ( 'NONE', #18168, #1159, #13817 ) ;
#1998 = ORIENTED_EDGE ( 'NONE', *, *, #9376, .F. ) ;
#1999 = ORIENTED_EDGE ( 'NONE', *, *, #10412, .F. ) ;
#2000 = ORIENTED_EDGE ( 'NONE', *, *, #11230, .T. ) ;
#2001 = CARTESIAN_POINT ( 'NONE',  ( -9.504075082187823043, -21.75730675493566579, 4.330127018922214077 ) ) ;
#2002 = ORIENTED_EDGE ( 'NONE', *, *, #6879, .F. ) ;
#2003 = EDGE_LOOP ( 'NONE', ( #14656, #16427, #4356, #15741 ) ) ;
#2004 = FACE_BOUND ( 'NONE', #13705, .T. ) ;
#2005 = EDGE_CURVE ( 'NONE', #8575, #3590, #2409, .T. ) ;
#2006 = EDGE_CURVE ( 'NONE', #9635, #8612, #18574, .T. ) ;
#2007 = CIRCLE ( 'NONE', #6566, 1.499999999999999556 ) ;
#2008 = CARTESIAN_POINT ( 'NONE',  ( -16.87183468716221313, -80.63143713290352821, -4.330127018922185655 ) ) ;
#2009 = ORIENTED_EDGE ( 'NONE', *, *, #15330, .T. ) ;
#2010 = AXIS2_PLACEMENT_3D ( 'NONE', #6527, #5288, #18111 ) ;
#2011 = ORIENTED_EDGE ( 'NONE', *, *, #15762, .T. ) ;
#2012 = PLANE ( 'NONE',  #13053 ) ;
#2013 = FACE_BOUND ( 'NONE', #15725, .T. ) ;
#2014 = ORIENTED_EDGE ( 'NONE', *, *, #11541, .T. ) ;
#2015 = DIRECTION ( 'NONE',  ( -0.1566598588826321192, 0.9876526153536342445, 7.798540720466731404E-17 ) ) ;
#2016 = CARTESIAN_POINT ( 'NONE',  ( -62.83731631128386397, -30.21693913459777647, 8.660254037844417496 ) ) ;
#2017 = AXIS2_PLACEMENT_3D ( 'NONE', #13064, #17448, #8977 ) ;
#2018 = DIRECTION ( 'NONE',  ( -0.1566598588826321192, 0.9876526153536342445, 7.798540720466730171E-17 ) ) ;
#2019 = ORIENTED_EDGE ( 'NONE', *, *, #12167, .T. ) ;
#2020 = ORIENTED_EDGE ( 'NONE', *, *, #6851, .F. ) ;
#2021 = DIRECTION ( 'NONE',  ( -0.9876526153536336894, -0.1566598588826349503, 0.000000000000000000 ) ) ;
#2022 = AXIS2_PLACEMENT_3D ( 'NONE', #7051, #8552, #2658 ) ;
#2023 = DIRECTION ( 'NONE',  ( 0.000000000000000000, 0.000000000000000000, 1.000000000000000000 ) ) ;
#2024 = ORIENTED_EDGE ( 'NONE', *, *, #7887, .T. ) ;
#2025 = VECTOR ( 'NONE', #9331, 1000.000000000000000 ) ;
#2026 = ORIENTED_EDGE ( 'NONE', *, *, #1905, .T. ) ;
#2027 = DIRECTION ( 'NONE',  ( 0.000000000000000000, 0.000000000000000000, 1.000000000000000000 ) ) ;
#2028 = AXIS2_PLACEMENT_3D ( 'NONE', #3381, #4808, #10494 ) ;
#2029 = ORIENTED_EDGE ( 'NONE', *, *, #18331, .F. ) ;
#2030 = FACE_BOUND ( 'NONE', #11289, .T. ) ;
#2031 = VECTOR ( 'NONE', #8879, 1000.000000000000000 ) ;
#2032 = CYLINDRICAL_SURFACE ( 'NONE', #16388, 1.500000000000001554 ) ;
#2033 = EDGE_CURVE ( 'NONE', #12526, #10470, #3073, .T. ) ;
#2034 = CARTESIAN_POINT ( 'NONE',  ( -58.84707083969148300, -87.28948113541535747, -17.32050807568878525 ) ) ;
#2035 = CARTESIAN_POINT ( 'NONE',  ( -172.7326993491721225, 43.83249341393818810, 9.951701414186830458E-16 ) ) ;
#2036 = CARTESIAN_POINT ( 'NONE',  ( -64.31879523431432233, -30.45192892292171294, -8.660254037844380193 ) ) ;
#2037 = EDGE_CURVE ( 'NONE', #11894, #9998, #61, .T. ) ;
#2038 = DIRECTION ( 'NONE',  ( 0.000000000000000000, 0.000000000000000000, 1.000000000000000000 ) ) ;
#2039 = DIRECTION ( 'NONE',  ( -0.1566598588826321747, 0.9876526153536343555, 0.000000000000000000 ) ) ;
#2040 = ORIENTED_EDGE ( 'NONE', *, *, #6876, .T. ) ;
#2041 = CARTESIAN_POINT ( 'NONE',  ( -77.65210554158829837, -32.56683701783724416, 1.869203119972154228E-14 ) ) ;
#2042 = EDGE_LOOP ( 'NONE', ( #8774, #10055 ) ) ;
#2043 = CIRCLE ( 'NONE', #16268, 1.500000000000001332 ) ;
#2044 = EDGE_LOOP ( 'NONE', ( #1599, #13275, #10107, #15945 ) ) ;
#2045 = LINE ( 'NONE', #4963, #7869 ) ;
#2046 = EDGE_LOOP ( 'NONE', ( #7736, #9894, #11498, #9115 ) ) ;
#2047 = FACE_OUTER_BOUND ( 'NONE', #12379, .T. ) ;
#2048 = DIRECTION ( 'NONE',  ( -0.1566598588826321192, 0.9876526153536342445, 7.798540720466730171E-17 ) ) ;
#2049 = VECTOR ( 'NONE', #15616, 1000.000000000000000 ) ;
#2050 = EDGE_LOOP ( 'NONE', ( #13470, #17687 ) ) ;
#2051 = DIRECTION ( 'NONE',  ( -0.1566598588826321192, 0.9876526153536342445, 7.798540720466730171E-17 ) ) ;
#2052 = EDGE_CURVE ( 'NONE', #16948, #9536, #17331, .T. ) ;
#2053 = DIRECTION ( 'NONE',  ( -0.1566598588826321192, 0.9876526153536342445, 7.798540720466731404E-17 ) ) ;
#2054 = CARTESIAN_POINT ( 'NONE',  ( -306.0881213225399051, -2.850701963179328668, 9.951701414186818625E-16 ) ) ;
#2055 = DIRECTION ( 'NONE',  ( -0.1566598588826321192, 0.9876526153536342445, 7.798540720466730171E-17 ) ) ;
#2056 = AXIS2_PLACEMENT_3D ( 'NONE', #9834, #14191, #14294 ) ;
#2057 = DIRECTION ( 'NONE',  ( -1.000000000000000000, 0.000000000000000000, 0.000000000000000000 ) ) ;
#2058 = CARTESIAN_POINT ( 'NONE',  ( -129.1404785418517918, -2.850701963179328668, 9.951701414186818625E-16 ) ) ;
#2059 = EDGE_CURVE ( 'NONE', #9632, #8678, #11526, .T. ) ;
#2060 = CIRCLE ( 'NONE', #15075, 1.500000000000000888 ) ;
#2061 = DIRECTION ( 'NONE',  ( -0.9876526153536336894, -0.1566598588826349503, 0.000000000000000000 ) ) ;
#2062 = CIRCLE ( 'NONE', #2401, 1.500000000000001332 ) ;
#2063 = VERTEX_POINT ( 'NONE', #17489 ) ;
#2064 = DIRECTION ( 'NONE',  ( 0.000000000000000000, 0.000000000000000000, 1.000000000000000000 ) ) ;
#2066 = ORIENTED_EDGE ( 'NONE', *, *, #16543, .T. ) ;
#2065 = DIRECTION ( 'NONE',  ( 1.000000000000000000, 0.000000000000000000, 0.000000000000000000 ) ) ;
#2067 = STYLED_ITEM ( 'NONE', ( #3832 ), #1868 ) ;
#2068 = DIRECTION ( 'NONE',  ( -0.3915338189555018222, -0.9201637183752250371, 0.000000000000000000 ) ) ;
#2069 = ORIENTED_EDGE ( 'NONE', *, *, #1068, .F. ) ;
#2070 = ORIENTED_EDGE ( 'NONE', *, *, #4867, .F. ) ;
#2071 = ORIENTED_EDGE ( 'NONE', *, *, #14640, .T. ) ;
#2072 = AXIS2_PLACEMENT_3D ( 'NONE', #7267, #5646, #8672 ) ;
#2073 = CARTESIAN_POINT ( 'NONE',  ( -172.7326993491721225, 43.83249341393818810, 9.951701414186830458E-16 ) ) ;
#2074 = VECTOR ( 'NONE', #10680, 1000.000000000000000 ) ;
#2075 = CARTESIAN_POINT ( 'NONE',  ( -14.40270314877813895, -80.23978748569695085, 17.32050807568881368 ) ) ;
#2076 = CIRCLE ( 'NONE', #9935, 1.499999999999999556 ) ;
#2077 = DIRECTION ( 'NONE',  ( 0.000000000000000000, 0.000000000000000000, -1.000000000000000000 ) ) ;
#2078 = CARTESIAN_POINT ( 'NONE',  ( -31.68662391746666884, -82.98133501614299234, -12.99038105676658539 ) ) ;
#2079 = PRODUCT_DEFINITION_CONTEXT ( 'detailed design', #18202, 'design' ) ;
#2080 = EDGE_CURVE ( 'NONE', #777, #11543, #1468, .T. ) ;
#2081 = EDGE_CURVE ( 'NONE', #4058, #3679, #7258, .T. ) ;
#2082 = CYLINDRICAL_SURFACE ( 'NONE', #10230, 13.99999999999999822 ) ;
#2083 = CARTESIAN_POINT ( 'NONE',  ( -90.00000000000000000, 34.99999999999999289, 35.00000000000000000 ) ) ;
#2084 = DIRECTION ( 'NONE',  ( 1.000000000000000000, 0.000000000000000000, 0.000000000000000000 ) ) ;
#2085 = EDGE_LOOP ( 'NONE', ( #16322, #13061, #14561, #14604 ) ) ;
#2086 = EDGE_CURVE ( 'NONE', #7797, #4310, #14869, .T. ) ;
#2087 = DIRECTION ( 'NONE',  ( -0.1566598588826321192, 0.9876526153536342445, 7.798540720466731404E-17 ) ) ;
#2088 = EDGE_CURVE ( 'NONE', #6604, #3989, #7634, .T. ) ;
#2089 = CARTESIAN_POINT ( 'NONE',  ( -35.67686938905902849, -25.90879301532540779, -4.330127018922181215 ) ) ;
#2090 = EDGE_CURVE ( 'NONE', #10127, #17419, #10160, .T. ) ;
#2091 = AXIS2_PLACEMENT_3D ( 'NONE', #1131, #4026, #8406 ) ;
#2092 = LINE ( 'NONE', #685, #10562 ) ;
#2093 = AXIS2_PLACEMENT_3D ( 'NONE', #11506, #17515, #3080 ) ;
#2094 = ORIENTED_EDGE ( 'NONE', *, *, #18316, .F. ) ;
#2095 = ORIENTED_EDGE ( 'NONE', *, *, #717, .F. ) ;
#2096 = VERTEX_POINT ( 'NONE', #10353 ) ;
#2097 = ORIENTED_EDGE ( 'NONE', *, *, #3220, .T. ) ;
#2098 = CARTESIAN_POINT ( 'NONE',  ( 55.85952145814821534, 6.938893903907228378E-15, 92.77853496600735639 ) ) ;
#2099 = FACE_BOUND ( 'NONE', #4289, .T. ) ;
#2100 = CIRCLE ( 'NONE', #6650, 139.0000000000000000 ) ;
#2101 = CARTESIAN_POINT ( 'NONE',  ( -2.057045456857760524, -78.28153924966404986, -4.330127018922185655 ) ) ;
#2102 = EDGE_CURVE ( 'NONE', #11883, #10248, #9436, .T. ) ;
#2103 = ADVANCED_FACE ( 'NONE', ( #18666 ), #5637, .F. ) ;
#2104 = CIRCLE ( 'NONE', #7820, 1.500000000000000444 ) ;
#2105 = CIRCLE ( 'NONE', #2707, 150.0000000000000000 ) ;
#2106 = DIRECTION ( 'NONE',  ( -0.1566598588826321192, 0.9876526153536342445, 7.798540720466731404E-17 ) ) ;
#2107 = ORIENTED_EDGE ( 'NONE', *, *, #2994, .F. ) ;
#2108 = CARTESIAN_POINT ( 'NONE',  ( -309.1404785418517918, -2.850701963179328668, 9.951701414186818625E-16 ) ) ;
#2109 = CARTESIAN_POINT ( 'NONE',  ( -66.78792677269838407, -30.84357857012830095, 4.330127018922217630 ) ) ;
#2110 = PRODUCT_DEFINITION ( 'UNKNOWN', '', #18444, #16492 ) ;
#2111 = EDGE_CURVE ( 'NONE', #4310, #7797, #10637, .T. ) ;
#2112 = AXIS2_PLACEMENT_3D ( 'NONE', #18330, #12284, #18124 ) ;
#2113 = CARTESIAN_POINT ( 'NONE',  ( -73.13054148225640461, 46.33205954274173877, -2.756412765970647882 ) ) ;
#2114 = DIRECTION ( 'NONE',  ( -1.000000000000000000, 0.000000000000000000, 0.000000000000000000 ) ) ;
#2115 = VERTEX_POINT ( 'NONE', #6107 ) ;
#2116 = ORIENTED_EDGE ( 'NONE', *, *, #2404, .T. ) ;
#2117 = DIRECTION ( 'NONE',  ( -0.1566598588826321192, 0.9876526153536342445, 7.798540720466731404E-17 ) ) ;
#2118 = CIRCLE ( 'NONE', #10280, 1.499999999999999556 ) ;
#2119 = CARTESIAN_POINT ( 'NONE',  ( -29.21749237908258223, -82.58968536893640078, 7.308518362537324739E-15 ) ) ;
#2120 = EDGE_LOOP ( 'NONE', ( #14336, #10632, #9227, #2656 ) ) ;
#2121 = AXIS2_PLACEMENT_3D ( 'NONE', #8067, #6961, #11086 ) ;
#2122 = AXIS2_PLACEMENT_3D ( 'NONE', #10418, #12980, #8826 ) ;
#2123 = CARTESIAN_POINT ( 'NONE',  ( -86.18478963674542115, 32.34879426031891114, 30.00000000000002842 ) ) ;
#2124 = CARTESIAN_POINT ( 'NONE',  ( -169.3344985746950044, 31.92300743893811088, 3.146712427857110583 ) ) ;
#2125 = CIRCLE ( 'NONE', #2745, 1.500000000000000444 ) ;
#2126 = CARTESIAN_POINT ( 'NONE',  ( 5.275328570166847961E-15, 2.200000000000001510, -20.00000000000000355 ) ) ;
#2127 = TOROIDAL_SURFACE ( 'NONE', #16361, 155.0000000000000284, 5.000000000000000000 ) ;
#2128 = CARTESIAN_POINT ( 'NONE',  ( 0.000000000000000000, 0.000000000000000000, 30.00000000000000000 ) ) ;
#2129 = CARTESIAN_POINT ( 'NONE',  ( -6.047290928450125946, -21.20899724884646531, 4.330127018922214077 ) ) ;
#2130 = AXIS2_PLACEMENT_3D ( 'NONE', #8647, #5896, #4371 ) ;
#2131 = DIRECTION ( 'NONE',  ( 0.000000000000000000, 0.000000000000000000, 1.000000000000000000 ) ) ;
#2132 = CARTESIAN_POINT ( 'NONE',  ( -175.0529311237955596, 56.11526690008648899, 2.500000000000000000 ) ) ;
#2133 = VECTOR ( 'NONE', #18684, 1000.000000000000114 ) ;
#2134 = EDGE_CURVE ( 'NONE', #5271, #6856, #10440, .T. ) ;
#2135 = DIRECTION ( 'NONE',  ( -1.000000000000000000, 0.000000000000000000, -0.000000000000000000 ) ) ;
#2136 = CIRCLE ( 'NONE', #42, 1.499999999999999556 ) ;
#2137 = DIRECTION ( 'NONE',  ( -0.9876526153536344665, -0.1566598588826304539, 0.000000000000000000 ) ) ;
#2138 = VERTEX_POINT ( 'NONE', #7622 ) ;
#2139 = VERTEX_POINT ( 'NONE', #18057 ) ;
#2140 = DIRECTION ( 'NONE',  ( -0.9876526153536344665, -0.1566598588826304539, 0.000000000000000000 ) ) ;
#2141 = ORIENTED_EDGE ( 'NONE', *, *, #13823, .F. ) ;
#2142 = EDGE_LOOP ( 'NONE', ( #16142, #208, #5298, #15919 ) ) ;
#2143 = ORIENTED_EDGE ( 'NONE', *, *, #8442, .F. ) ;
#2144 = VERTEX_POINT ( 'NONE', #4755 ) ;
#2145 = EDGE_CURVE ( 'NONE', #1209, #3494, #5512, .T. ) ;
#2146 = CARTESIAN_POINT ( 'NONE',  ( 0.000000000000000000, 0.000000000000000000, 35.00000000000000000 ) ) ;
#2147 = CIRCLE ( 'NONE', #13934, 2.200000000000000178 ) ;
#2148 = ORIENTED_EDGE ( 'NONE', *, *, #4321, .T. ) ;
#2149 = EDGE_LOOP ( 'NONE', ( #13958, #11494, #17524, #16764 ) ) ;
#2150 = FACE_OUTER_BOUND ( 'NONE', #2085, .T. ) ;
#2151 = CARTESIAN_POINT ( 'NONE',  ( -23.29157668696081629, -81.64972621564064070, -4.330127018922185655 ) ) ;
#2152 = VECTOR ( 'NONE', #18373, 1000.000000000000000 ) ;
#2153 = DIRECTION ( 'NONE',  ( 1.000000000000000000, 0.000000000000000000, -0.000000000000000000 ) ) ;
#2154 = DIRECTION ( 'NONE',  ( -0.1615579233078772992, -0.9868632313631134911, 0.000000000000000000 ) ) ;
#2155 = DIRECTION ( 'NONE',  ( -0.1566598588826321192, 0.9876526153536342445, 7.798540720466730171E-17 ) ) ;
#2156 = DIRECTION ( 'NONE',  ( -1.000000000000000000, 0.000000000000000000, 0.000000000000000000 ) ) ;
#2157 = FILL_AREA_STYLE_COLOUR ( '', #6322 ) ;
#2158 = AXIS2_PLACEMENT_3D ( 'NONE', #7119, #12950, #4341 ) ;
#2159 = CARTESIAN_POINT ( 'NONE',  ( -83.14047854185180597, 6.938893903907228378E-15, 92.77853496600735639 ) ) ;
#2160 = FACE_OUTER_BOUND ( 'NONE', #13539, .T. ) ;
#2161 = FACE_BOUND ( 'NONE', #7843, .T. ) ;
#2162 = DIRECTION ( 'NONE',  ( 0.000000000000000000, 0.000000000000000000, -1.000000000000000000 ) ) ;
#2163 = CIRCLE ( 'NONE', #7624, 1.500000000000000888 ) ;
#2164 = DIRECTION ( 'NONE',  ( -0.1566598588826321192, 0.9876526153536342445, 7.798540720466730171E-17 ) ) ;
#2166 = ORIENTED_EDGE ( 'NONE', *, *, #1186, .F. ) ;
#2165 = DIRECTION ( 'NONE',  ( -0.9876526153536336894, -0.1566598588826350336, 0.000000000000000000 ) ) ;
#2167 = DIRECTION ( 'NONE',  ( 0.000000000000000000, 0.000000000000000000, 1.000000000000000000 ) ) ;
#2168 = EDGE_CURVE ( 'NONE', #9109, #8230, #8227, .T. ) ;
#2169 = EDGE_LOOP ( 'NONE', ( #12654, #9944, #4667, #8189 ) ) ;
#2170 = AXIS2_PLACEMENT_3D ( 'NONE', #6483, #12220, #9409 ) ;
#2171 = CARTESIAN_POINT ( 'NONE',  ( 0.000000000000000000, 0.000000000000000000, -20.00000000000000355 ) ) ;
#2172 = ADVANCED_FACE ( 'NONE', ( #10535 ), #2012, .F. ) ;
#2173 = ORIENTED_EDGE ( 'NONE', *, *, #6910, .F. ) ;
#2174 = AXIS2_PLACEMENT_3D ( 'NONE', #12078, #3652, #16476 ) ;
#2175 = CARTESIAN_POINT ( 'NONE',  ( -30.04042668367358360, -19.95224085582017537, 12.99038105676661736 ) ) ;
#2176 = ORIENTED_EDGE ( 'NONE', *, *, #11265, .F. ) ;
#2177 = DIRECTION ( 'NONE',  ( -0.1566598588826321747, 0.9876526153536343555, 0.000000000000000000 ) ) ;
#2178 = DIRECTION ( 'NONE',  ( 0.000000000000000000, 0.000000000000000000, 1.000000000000000000 ) ) ;
#2179 = CARTESIAN_POINT ( 'NONE',  ( -22.34355908178503469, -23.79388492040988012, -4.330127018922181215 ) ) ;
#2180 = CARTESIAN_POINT ( 'NONE',  ( -1.892327146095121204, -15.48743487766515337, 12.99038105676661026 ) ) ;
#2181 = EDGE_LOOP ( 'NONE', ( #18565, #13788, #12286, #17679 ) ) ;
#2182 = AXIS2_PLACEMENT_3D ( 'NONE', #13926, #14976, #5224 ) ;
#2183 = LINE ( 'NONE', #7963, #14898 ) ;
#2184 = DIRECTION ( 'NONE',  ( -0.1566598588826321747, 0.9876526153536343555, 0.000000000000000000 ) ) ;
#2185 = CYLINDRICAL_SURFACE ( 'NONE', #8168, 1.500000000000000666 ) ;
#2186 = CARTESIAN_POINT ( 'NONE',  ( -64.77298653181324539, -88.22944028871116018, -12.99038105676658539 ) ) ;
#2187 = AXIS2_PLACEMENT_3D ( 'NONE', #368, #14852, #10583 ) ;
#2188 = ORIENTED_EDGE ( 'NONE', *, *, #15045, .F. ) ;
#2189 = VERTEX_POINT ( 'NONE', #2199 ) ;
#2190 = ORIENTED_EDGE ( 'NONE', *, *, #3347, .T. ) ;
#2191 = CARTESIAN_POINT ( 'NONE',  ( -69.54653129781877396, -26.21863521112544149, 12.99038105676661736 ) ) ;
#2192 = EDGE_CURVE ( 'NONE', #13410, #16508, #13653, .T. ) ;
#2193 = EDGE_CURVE ( 'NONE', #11968, #1456, #15488, .T. ) ;
#2194 = FACE_BOUND ( 'NONE', #10461, .T. ) ;
#2195 = EDGE_CURVE ( 'NONE', #3989, #6604, #16099, .T. ) ;
#2196 = FILL_AREA_STYLE ('',( #9865 ) ) ;
#2197 = ORIENTED_EDGE ( 'NONE', *, *, #2667, .T. ) ;
#2198 = ORIENTED_EDGE ( 'NONE', *, *, #8033, .F. ) ;
#2199 = CARTESIAN_POINT ( 'NONE',  ( -0.9046745307415022808, -15.33077501878252136, 1.387778780781445518E-14 ) ) ;
#2200 = FACE_BOUND ( 'NONE', #1915, .T. ) ;
#2201 = DIRECTION ( 'NONE',  ( -0.9201637183752250371, 0.3915338189555017667, 2.458192809297184296E-16 ) ) ;
#2202 = DIRECTION ( 'NONE',  ( -0.000000000000000000, -0.000000000000000000, -1.000000000000000000 ) ) ;
#2203 = DIRECTION ( 'NONE',  ( -0.9876526153536336894, -0.1566598588826349503, 0.000000000000000000 ) ) ;
#2204 = FACE_OUTER_BOUND ( 'NONE', #5437, .T. ) ;
#2205 = ORIENTED_EDGE ( 'NONE', *, *, #10209, .F. ) ;
#2206 = ORIENTED_EDGE ( 'NONE', *, *, #18096, .T. ) ;
#2207 = CARTESIAN_POINT ( 'NONE',  ( -29.25712738926042888, -24.89050393258829175, 4.330127018922217630 ) ) ;
#2208 = ADVANCED_FACE ( 'NONE', ( #8277 ), #7046, .T. ) ;
#2209 = EDGE_CURVE ( 'NONE', #4027, #10083, #12700, .T. ) ;
#2210 = DIRECTION ( 'NONE',  ( -0.9876526153536336894, -0.1566598588826349503, 0.000000000000000000 ) ) ;
#2211 = ORIENTED_EDGE ( 'NONE', *, *, #18409, .T. ) ;
#2212 = ORIENTED_EDGE ( 'NONE', *, *, #9806, .T. ) ;
#2213 = DIRECTION ( 'NONE',  ( -0.9876526153536336894, -0.1566598588826349503, 0.000000000000000000 ) ) ;
#2214 = ADVANCED_FACE ( 'NONE', ( #13941 ), #16722, .F. ) ;
#2215 = CIRCLE ( 'NONE', #14013, 1.500000000000000000 ) ;
#2216 = ORIENTED_EDGE ( 'NONE', *, *, #5344, .F. ) ;
#2217 = DIRECTION ( 'NONE',  ( 0.000000000000000000, 0.000000000000000000, 1.000000000000000000 ) ) ;
#2218 = VERTEX_POINT ( 'NONE', #7980 ) ;
#2219 = FACE_BOUND ( 'NONE', #4988, .T. ) ;
#2220 = CARTESIAN_POINT ( 'NONE',  ( -15.71946376104596155, -17.68067290202200326, 8.660254037844413944 ) ) ;
#2221 = CARTESIAN_POINT ( 'NONE',  ( 2.841582609732560272, -19.79905851890276836, 17.32050807568881012 ) ) ;
#2222 = DIRECTION ( 'NONE',  ( 1.000000000000000000, 0.000000000000000000, 0.000000000000000000 ) ) ;
#2223 =( NAMED_UNIT ( * ) PLANE_ANGLE_UNIT ( ) SI_UNIT ( $, .RADIAN. ) );
#2224 = VERTEX_POINT ( 'NONE', #786 ) ;
#2225 = AXIS2_PLACEMENT_3D ( 'NONE', #3368, #16274, #10389 ) ;
#2226 = DIRECTION ( 'NONE',  ( -0.1566598588826321192, 0.9876526153536342445, 7.798540720466730171E-17 ) ) ;
#2227 = SURFACE_STYLE_FILL_AREA ( #15211 ) ;
#2228 = PLANE ( 'NONE',  #7808 ) ;
#2229 = CARTESIAN_POINT ( 'NONE',  ( -48.80582637539254875, -22.92877817459017109, 8.660254037844417496 ) ) ;
#2230 = EDGE_LOOP ( 'NONE', ( #5491, #7299 ) ) ;
#2231 = ORIENTED_EDGE ( 'NONE', *, *, #18528, .T. ) ;
#2232 = CARTESIAN_POINT ( 'NONE',  ( -79.20163718375225415, 48.91533818955501545, 2.500000000000000000 ) ) ;
#2233 = ORIENTED_EDGE ( 'NONE', *, *, #10295, .F. ) ;
#2234 = ORIENTED_EDGE ( 'NONE', *, *, #14306, .T. ) ;
#2235 = ORIENTED_EDGE ( 'NONE', *, *, #9131, .T. ) ;
#2236 = CYLINDRICAL_SURFACE ( 'NONE', #2325, 1.500000000000001554 ) ;
#2237 = CARTESIAN_POINT ( 'NONE',  ( -55.22556837519117323, -23.94706725732726582, -17.32050807568878170 ) ) ;
#2238 = EDGE_CURVE ( 'NONE', #719, #5148, #6855, .T. ) ;
#2239 = CARTESIAN_POINT ( 'NONE',  ( -54.89646037827696290, -86.66284169988483654, 4.330127018922213189 ) ) ;
#2240 = EDGE_CURVE ( 'NONE', #6731, #15683, #12755, .T. ) ;
#2241 = DIRECTION ( 'NONE',  ( 0.000000000000000000, 0.000000000000000000, 1.000000000000000000 ) ) ;
#2242 = ORIENTED_EDGE ( 'NONE', *, *, #17053, .F. ) ;
#2243 = CARTESIAN_POINT ( 'NONE',  ( -39.13365354279672914, -26.45710252141460828, 21.65063509461101887 ) ) ;
#2244 = EDGE_CURVE ( 'NONE', #14517, #4155, #11239, .T. ) ;
#2245 = CARTESIAN_POINT ( 'NONE',  ( -46.50141314777108903, -85.33123289938248490, 21.65063509461101532 ) ) ;
#2246 = DIRECTION ( 'NONE',  ( -0.1566598588826321192, 0.9876526153536342445, 7.798540720466731404E-17 ) ) ;
#2247 = DIRECTION ( 'NONE',  ( 0.000000000000000000, -1.000000000000000000, 0.000000000000000000 ) ) ;
#2248 = CARTESIAN_POINT ( 'NONE',  ( -84.20837060243641758, 32.64545563739221024, 35.00000599999999906 ) ) ;
#2249 = EDGE_LOOP ( 'NONE', ( #4015, #2353 ) ) ;
#2250 = FACE_OUTER_BOUND ( 'NONE', #9511, .T. ) ;
#2251 = AXIS2_PLACEMENT_3D ( 'NONE', #18612, #15600, #12407 ) ;
#2252 = ORIENTED_EDGE ( 'NONE', *, *, #4677, .F. ) ;
#2253 = ORIENTED_EDGE ( 'NONE', *, *, #4651, .T. ) ;
#2254 = CARTESIAN_POINT ( 'NONE',  ( -50.28730529842300001, -23.16376796291411821, 8.660254037844417496 ) ) ;
#2255 = EDGE_LOOP ( 'NONE', ( #8646, #9606, #6691, #1107 ) ) ;
#2256 = DIRECTION ( 'NONE',  ( -0.1566598588826321192, 0.9876526153536342445, 7.798540720466731404E-17 ) ) ;
#2257 = CARTESIAN_POINT ( 'NONE',  ( -12.75650591498505371, -17.21069332537410901, -17.32050807568878170 ) ) ;
#2258 = EDGE_LOOP ( 'NONE', ( #12744, #14922, #1094, #12317 ) ) ;
#2259 = CARTESIAN_POINT ( 'NONE',  ( -31.68662391746665463, -82.98133501614299234, -4.330127018922185655 ) ) ;
#2260 = CARTESIAN_POINT ( 'NONE',  ( -80.88842949533930948, 2.743677230443736903, -2.574918967431987227 ) ) ;
#2261 = EDGE_CURVE ( 'NONE', #18705, #11379, #4589, .T. ) ;
#2262 = CARTESIAN_POINT ( 'NONE',  ( 1.360103686702108128, -20.03404830722672259, 1.348786077179111942E-14 ) ) ;
#2263 = CIRCLE ( 'NONE', #18053, 2.000000000000001776 ) ;
#2264 = DIRECTION ( 'NONE',  ( -1.000000000000000000, 0.000000000000000000, 0.000000000000000000 ) ) ;
#2265 = DIRECTION ( 'NONE',  ( -0.1566598588826321192, 0.9876526153536342445, 7.798540720466730171E-17 ) ) ;
#2266 = EDGE_LOOP ( 'NONE', ( #6257, #16011 ) ) ;
#2267 = FACE_BOUND ( 'NONE', #167, .T. ) ;
#2268 = DIRECTION ( 'NONE',  ( -0.9826218788918642533, -0.1856185419698762884, 0.000000000000000000 ) ) ;
#2269 = DIRECTION ( 'NONE',  ( 0.000000000000000000, 0.000000000000000000, 1.000000000000000000 ) ) ;
#2270 = DIRECTION ( 'NONE',  ( -0.9876526153536341335, -0.1566598588826327021, 0.000000000000000000 ) ) ;
#2271 = EDGE_CURVE ( 'NONE', #17176, #14148, #5818, .T. ) ;
#2272 = FACE_OUTER_BOUND ( 'NONE', #18170, .T. ) ;
#2273 = ORIENTED_EDGE ( 'NONE', *, *, #3881, .T. ) ;
#2274 = ORIENTED_EDGE ( 'NONE', *, *, #11748, .T. ) ;
#2275 = EDGE_LOOP ( 'NONE', ( #3398, #12045, #9731, #10897 ) ) ;
#2276 = FACE_BOUND ( 'NONE', #7402, .T. ) ;
#2277 = VECTOR ( 'NONE', #6489, 1000.000000000000000 ) ;
#2278 = FACE_BOUND ( 'NONE', #7998, .T. ) ;
#2279 = VERTEX_POINT ( 'NONE', #12517 ) ;
#2280 = CARTESIAN_POINT ( 'NONE',  ( -6.995308533625909320, -79.06483854407721878, 12.99038105676660848 ) ) ;
#2281 = CIRCLE ( 'NONE', #3780, 1.500000000000000000 ) ;
#2282 = EDGE_CURVE ( 'NONE', #14381, #16999, #10900, .T. ) ;
#2283 = DIRECTION ( 'NONE',  ( -0.1566598588826321192, 0.9876526153536342445, 7.798540720466730171E-17 ) ) ;
#2284 = FACE_BOUND ( 'NONE', #18682, .T. ) ;
#2285 = FACE_OUTER_BOUND ( 'NONE', #5660, .T. ) ;
#2286 = VERTEX_POINT ( 'NONE', #9703 ) ;
#2287 = AXIS2_PLACEMENT_3D ( 'NONE', #14317, #1342, #7124 ) ;
#2288 = LINE ( 'NONE', #4935, #4220 ) ;
#2289 = EDGE_CURVE ( 'NONE', #7636, #3282, #2491, .T. ) ;
#2290 = LINE ( 'NONE', #8071, #9863 ) ;
#2291 = ORIENTED_EDGE ( 'NONE', *, *, #15337, .T. ) ;
#2292 = EDGE_LOOP ( 'NONE', ( #4470, #14480 ) ) ;
#2293 = CYLINDRICAL_SURFACE ( 'NONE', #8428, 1.500000000000001554 ) ;
#2294 = ORIENTED_EDGE ( 'NONE', *, *, #4880, .F. ) ;
#2295 = CARTESIAN_POINT ( 'NONE',  ( -169.9074338689577530, 31.96868808717145782, -3.724467847532850762 ) ) ;
#2296 = ORIENTED_EDGE ( 'NONE', *, *, #15182, .F. ) ;
#2297 = ORIENTED_EDGE ( 'NONE', *, *, #9033, .F. ) ;
#2298 = FACE_OUTER_BOUND ( 'NONE', #4277, .T. ) ;
#2299 = AXIS2_PLACEMENT_3D ( 'NONE', #6386, #8924, #10627 ) ;
#2300 = VERTEX_POINT ( 'NONE', #3980 ) ;
#2301 = CARTESIAN_POINT ( 'NONE',  ( -127.1354840320379225, -15.28154141549707035, 2.662644313562638310 ) ) ;
#2302 = AXIS2_PLACEMENT_3D ( 'NONE', #16083, #8408, #15979 ) ;
#2303 = CYLINDRICAL_SURFACE ( 'NONE', #1831, 1.500000000000001554 ) ;
#2304 = CARTESIAN_POINT ( 'NONE',  ( -51.27495791377663181, -23.32042782179674489, -4.330127018922180326 ) ) ;
#2305 = CARTESIAN_POINT ( 'NONE',  ( -74.62210677719829732, 46.96672731380024146, 2.500000000000000000 ) ) ;
#2306 = CARTESIAN_POINT ( 'NONE',  ( 0.000000000000000000, 0.000000000000000000, 0.000000000000000000 ) ) ;
#2307 = EDGE_CURVE ( 'NONE', #4718, #4101, #9786, .T. ) ;
#2308 = ADVANCED_FACE ( 'NONE', ( #4070 ), #13740, .F. ) ;
#2309 = ADVANCED_FACE ( 'NONE', ( #7040 ), #11261, .F. ) ;
#2310 = AXIS2_PLACEMENT_3D ( 'NONE', #3116, #8905, #17744 ) ;
#2311 = FACE_OUTER_BOUND ( 'NONE', #5865, .T. ) ;
#2312 = CARTESIAN_POINT ( 'NONE',  ( -42.38608437559395981, -21.91048909185306215, -8.660254037844380193 ) ) ;
#2313 = ADVANCED_FACE ( 'NONE', ( #12784 ), #18629, .F. ) ;
#2314 = DIRECTION ( 'NONE',  ( 0.000000000000000000, 1.000000000000000000, 1.224646799147353207E-16 ) ) ;
#2315 = ORIENTED_EDGE ( 'NONE', *, *, #14957, .T. ) ;
#2316 = EDGE_LOOP ( 'NONE', ( #14529, #15736, #9747, #13850 ) ) ;
#2317 = FACE_BOUND ( 'NONE', #14050, .T. ) ;
#2318 = CARTESIAN_POINT ( 'NONE',  ( -67.73594437787414790, -88.69941986535906153, -4.330127018922185655 ) ) ;
#2319 = VERTEX_POINT ( 'NONE', #15724 ) ;
#2320 = CARTESIAN_POINT ( 'NONE',  ( -9.464440072009985272, -79.45648819128378193, -8.660254037844385522 ) ) ;
#2321 = ORIENTED_EDGE ( 'NONE', *, *, #3926, .T. ) ;
#2322 = ORIENTED_EDGE ( 'NONE', *, *, #16408, .T. ) ;
#2323 = CARTESIAN_POINT ( 'NONE',  ( -10.45209268736360997, -79.61314805016640150, -21.65063509461098690 ) ) ;
#2324 = AXIS2_PLACEMENT_3D ( 'NONE', #15019, #4685, #438 ) ;
#2325 = AXIS2_PLACEMENT_3D ( 'NONE', #18306, #16771, #8116 ) ;
#2326 = CARTESIAN_POINT ( 'NONE',  ( -3.373806069125583562, -15.72242466598909871, -21.65063509461098334 ) ) ;
#2327 = DIRECTION ( 'NONE',  ( -0.9876526153536336894, -0.1566598588826349503, 0.000000000000000000 ) ) ;
#2328 = VERTEX_POINT ( 'NONE', #9674 ) ;
#2329 = PLANE ( 'NONE',  #12706 ) ;
#2330 = DIRECTION ( 'NONE',  ( -0.1566598588826321747, 0.9876526153536343555, 0.000000000000000000 ) ) ;
#2331 = CIRCLE ( 'NONE', #3829, 1.499999999999999556 ) ;
#2332 = PRESENTATION_LAYER_ASSIGNMENT (  '', '', ( #10198 ) ) ;
#2333 = DIRECTION ( 'NONE',  ( -0.1566598588826321192, 0.9876526153536342445, 7.798540720466730171E-17 ) ) ;
#2334 = ADVANCED_FACE ( 'NONE', ( #18343 ), #2747, .F. ) ;
#2335 = EDGE_CURVE ( 'NONE', #6102, #10673, #6118, .T. ) ;
#2336 = CARTESIAN_POINT ( 'NONE',  ( -49.59961335071795929, 37.20051552679455398, 20.00000000000001066 ) ) ;
#2337 = CARTESIAN_POINT ( 'NONE',  ( -67.57122606711153878, -25.90531549336017392, 12.99038105676661736 ) ) ;
#2338 = CIRCLE ( 'NONE', #13524, 1.500000000000001332 ) ;
#2339 = DIRECTION ( 'NONE',  ( -0.9876526153536336894, -0.1566598588826350336, 0.000000000000000000 ) ) ;
#2340 = ORIENTED_EDGE ( 'NONE', *, *, #14918, .T. ) ;
#2341 = EDGE_CURVE ( 'NONE', #18706, #11180, #17027, .T. ) ;
#2342 = FACE_OUTER_BOUND ( 'NONE', #4630, .T. ) ;
#2343 = ORIENTED_EDGE ( 'NONE', *, *, #7518, .F. ) ;
#2344 = CYLINDRICAL_SURFACE ( 'NONE', #15747, 1.500000000000001554 ) ;
#2345 = EDGE_LOOP ( 'NONE', ( #17280, #16458, #17068, #1845 ) ) ;
#2346 = AXIS2_PLACEMENT_3D ( 'NONE', #7532, #6313, #9144 ) ;
#2347 = ORIENTED_EDGE ( 'NONE', *, *, #17236, .F. ) ;
#2348 = CARTESIAN_POINT ( 'NONE',  ( -62.83731631128386397, -30.21693913459777647, 1.869203119972154228E-14 ) ) ;
#2349 = ORIENTED_EDGE ( 'NONE', *, *, #15969, .F. ) ;
#2350 = CARTESIAN_POINT ( 'NONE',  ( -1.069392841504132052, -78.12487939078141608, -8.660254037844385522 ) ) ;
#2351 = VERTEX_POINT ( 'NONE', #5911 ) ;
#2352 = CYLINDRICAL_SURFACE ( 'NONE', #6764, 2.000000000000000000 ) ;
#2353 = ORIENTED_EDGE ( 'NONE', *, *, #2088, .F. ) ;
#2354 = DIRECTION ( 'NONE',  ( 0.000000000000000000, 0.000000000000000000, 1.000000000000000000 ) ) ;
#2355 = CARTESIAN_POINT ( 'NONE',  ( 5.350349158294472218, -77.10659030804430358, 1.077796531449093893E-14 ) ) ;
#2356 = AXIS2_PLACEMENT_3D ( 'NONE', #17243, #10657, #16172 ) ;
#2357 = CARTESIAN_POINT ( 'NONE',  ( 0.3724510713484854851, -20.19070816610934926, -12.99038105676658361 ) ) ;
#2358 = DIRECTION ( 'NONE',  ( -0.1566598588826321192, 0.9876526153536342445, 7.798540720466730171E-17 ) ) ;
#2359 = CARTESIAN_POINT ( 'NONE',  ( -69.99999999999998579, -45.00000000000000711, 25.00000000000000000 ) ) ;
#2360 = VECTOR ( 'NONE', #90, 1000.000000000000000 ) ;
#2361 = DIRECTION ( 'NONE',  ( -0.9876526153536341335, -0.1566598588826327021, 0.000000000000000000 ) ) ;
#2362 = EDGE_CURVE ( 'NONE', #7723, #795, #18279, .T. ) ;
#2363 = CARTESIAN_POINT ( 'NONE',  ( 5.350349158294472218, -77.10659030804430358, -17.32050807568878525 ) ) ;
#2364 = EDGE_CURVE ( 'NONE', #14520, #17136, #12030, .T. ) ;
#2365 = AXIS2_PLACEMENT_3D ( 'NONE', #3427, #17888, #6406 ) ;
#2366 = ORIENTED_EDGE ( 'NONE', *, *, #10826, .F. ) ;
#2367 = ORIENTED_EDGE ( 'NONE', *, *, #7350, .F. ) ;
#2368 = ORIENTED_EDGE ( 'NONE', *, *, #980, .F. ) ;
#2369 = ORIENTED_EDGE ( 'NONE', *, *, #18134, .T. ) ;
#2370 = CARTESIAN_POINT ( 'NONE',  ( -11.93357161039406300, -79.84813783849037350, 4.330127018922213189 ) ) ;
#2371 = CIRCLE ( 'NONE', #13861, 2.000000000000001776 ) ;
#2372 = EDGE_CURVE ( 'NONE', #14394, #2138, #11538, .T. ) ;
#2373 = CIRCLE ( 'NONE', #18770, 1.500000000000001332 ) ;
#2374 = FACE_BOUND ( 'NONE', #11193, .T. ) ;
#2375 = CIRCLE ( 'NONE', #16922, 1.500000000000000888 ) ;
#2376 = LINE ( 'NONE', #3779, #12779 ) ;
#2377 = CIRCLE ( 'NONE', #5418, 2.000000000000000000 ) ;
#2378 = TOROIDAL_SURFACE ( 'NONE', #5096, 3.000000000000000000, 2.000000000000000000 ) ;
#2379 = CARTESIAN_POINT ( 'NONE',  ( -8.476787456656362352, -79.29982833240116236, 4.330127018922213189 ) ) ;
#2380 = AXIS2_PLACEMENT_3D ( 'NONE', #7309, #11620, #1688 ) ;
#2381 = CARTESIAN_POINT ( 'NONE',  ( 3.000000000000004441, 4.898587196589418745E-16, -22.00000000000000711 ) ) ;
#2382 = DIRECTION ( 'NONE',  ( -1.000000000000000000, 0.000000000000000000, -1.435633221498047038E-16 ) ) ;
#2383 = CIRCLE ( 'NONE', #12356, 1.500000000000000888 ) ;
#2384 = ORIENTED_EDGE ( 'NONE', *, *, #7202, .T. ) ;
#2385 = CARTESIAN_POINT ( 'NONE',  ( -75.96627329761737712, -27.23692429386253977, 4.330127018922218518 ) ) ;
#2386 = DIRECTION ( 'NONE',  ( -0.1566598588826321192, 0.9876526153536342445, 7.798540720466731404E-17 ) ) ;
#2387 = DIRECTION ( 'NONE',  ( 0.000000000000000000, 0.000000000000000000, 1.000000000000000000 ) ) ;
#2388 = CARTESIAN_POINT ( 'NONE',  ( -58.88670584986932965, -29.59029969906724844, 4.330127018922217630 ) ) ;
#2389 = CARTESIAN_POINT ( 'NONE',  ( -170.5980861165185445, 32.53234180668174247, -5.500000000000001776 ) ) ;
#2390 = VERTEX_POINT ( 'NONE', #11928 ) ;
#2391 = CIRCLE ( 'NONE', #11755, 1.500000000000000444 ) ;
#2392 = ORIENTED_EDGE ( 'NONE', *, *, #9208, .F. ) ;
#2393 = CYLINDRICAL_SURFACE ( 'NONE', #5847, 1.500000000000001554 ) ;
#2394 = ADVANCED_FACE ( 'NONE', ( #4758 ), #17779, .F. ) ;
#2395 = CIRCLE ( 'NONE', #15711, 1.500000000000000888 ) ;
#2396 = ORIENTED_EDGE ( 'NONE', *, *, #18794, .T. ) ;
#2397 = ORIENTED_EDGE ( 'NONE', *, *, #5880, .F. ) ;
#2398 = CYLINDRICAL_SURFACE ( 'NONE', #10023, 1.500000000000001554 ) ;
#2399 = DIRECTION ( 'NONE',  ( -0.1566598588826321747, 0.9876526153536343555, 0.000000000000000000 ) ) ;
#2400 = CIRCLE ( 'NONE', #6347, 1.500000000000000000 ) ;
#2401 = AXIS2_PLACEMENT_3D ( 'NONE', #4129, #2728, #15985 ) ;
#2402 = AXIS2_PLACEMENT_3D ( 'NONE', #4373, #10060, #7065 ) ;
#2403 = FACE_BOUND ( 'NONE', #10267, .T. ) ;
#2404 = EDGE_CURVE ( 'NONE', #10467, #6767, #3682, .T. ) ;
#2405 = CARTESIAN_POINT ( 'NONE',  ( 55.85952145814821534, 6.938893903907228378E-15, 35.00000000000000000 ) ) ;
#2406 = EDGE_CURVE ( 'NONE', #11338, #2916, #10344, .T. ) ;
#2407 = DIRECTION ( 'NONE',  ( 0.000000000000000000, 0.000000000000000000, 1.000000000000000000 ) ) ;
#2408 = CARTESIAN_POINT ( 'NONE',  ( -72.99658078354744362, 46.27505866028131010, 2.816616659167352044 ) ) ;
#2409 = LINE ( 'NONE', #11012, #5208 ) ;
#2410 = DIRECTION ( 'NONE',  ( 0.000000000000000000, 0.000000000000000000, 1.000000000000000000 ) ) ;
#2411 = CIRCLE ( 'NONE', #12385, 1.499999999999999556 ) ;
#2412 = LINE ( 'NONE', #8380, #9979 ) ;
#2414 = CARTESIAN_POINT ( 'NONE',  ( -41.56315007100297265, -84.54793360496931598, -12.99038105676658539 ) ) ;
#2413 = AXIS2_PLACEMENT_3D ( 'NONE', #10642, #17598, #6205 ) ;
#2415 = ORIENTED_EDGE ( 'NONE', *, *, #16291, .F. ) ;
#2416 = CARTESIAN_POINT ( 'NONE',  ( -51.97313754239392836, -28.49368068688882971, 4.330127018922217630 ) ) ;
#2417 = CARTESIAN_POINT ( 'NONE',  ( -1.892327146095121204, -15.48743487766515337, 4.330127018922213189 ) ) ;
#2418 = VECTOR ( 'NONE', #15957, 1000.000000000000000 ) ;
#2419 = ORIENTED_EDGE ( 'NONE', *, *, #3895, .T. ) ;
#2420 = VERTEX_POINT ( 'NONE', #15930 ) ;
#2421 = CARTESIAN_POINT ( 'NONE',  ( -84.20837060243641758, 32.64545563739221024, 35.00000599999999906 ) ) ;
#2422 = CIRCLE ( 'NONE', #13007, 5.000000000000000000 ) ;
#2423 = VERTEX_POINT ( 'NONE', #9108 ) ;
#2424 = ORIENTED_EDGE ( 'NONE', *, *, #16634, .T. ) ;
#2425 = FACE_OUTER_BOUND ( 'NONE', #6337, .T. ) ;
#2426 = CYLINDRICAL_SURFACE ( 'NONE', #13314, 1.500000000000000666 ) ;
#2427 = ORIENTED_EDGE ( 'NONE', *, *, #11947, .T. ) ;
#2428 = DIRECTION ( 'NONE',  ( -0.1566598588826321747, 0.9876526153536343555, 0.000000000000000000 ) ) ;
#2429 = CARTESIAN_POINT ( 'NONE',  ( -62.83731631128386397, -30.21693913459777647, -17.32050807568878170 ) ) ;
#2430 = VECTOR ( 'NONE', #835, 1000.000000000000000 ) ;
#2431 = ADVANCED_FACE ( 'NONE', ( #3042 ), #14693, .F. ) ;
#2432 = EDGE_CURVE ( 'NONE', #3894, #8207, #1712, .T. ) ;
#2433 = VECTOR ( 'NONE', #2164, 1000.000000000000000 ) ;
#2434 = DIRECTION ( 'NONE',  ( -0.1566598588826321747, 0.9876526153536343555, 0.000000000000000000 ) ) ;
#2435 = CYLINDRICAL_SURFACE ( 'NONE', #18191, 1.500000000000000666 ) ;
#2436 = EDGE_CURVE ( 'NONE', #15692, #14720, #2938, .T. ) ;
#2437 = ORIENTED_EDGE ( 'NONE', *, *, #16111, .T. ) ;
#2438 = VECTOR ( 'NONE', #12223, 1000.000000000000000 ) ;
#2439 = FACE_OUTER_BOUND ( 'NONE', #4415, .T. ) ;
#2440 = CARTESIAN_POINT ( 'NONE',  ( -2.000000000000000000, 0.000000000000000000, 30.00000000000000000 ) ) ;
#2441 = DIRECTION ( 'NONE',  ( 0.1856185419698762884, -0.9826218788918642533, 0.000000000000000000 ) ) ;
#2442 = VECTOR ( 'NONE', #5275, 1000.000000000000000 ) ;
#2443 = FACE_OUTER_BOUND ( 'NONE', #18447, .T. ) ;
#2444 = DIRECTION ( 'NONE',  ( -0.1566598588826321747, 0.9876526153536343555, 0.000000000000000000 ) ) ;
#2445 = ORIENTED_EDGE ( 'NONE', *, *, #7202, .F. ) ;
#2446 = DIRECTION ( 'NONE',  ( 0.000000000000000000, 0.000000000000000000, 1.000000000000000000 ) ) ;
#2447 = EDGE_LOOP ( 'NONE', ( #5086, #2274, #17953, #17450 ) ) ;
#2448 = ORIENTED_EDGE ( 'NONE', *, *, #16132, .T. ) ;
#2449 = CARTESIAN_POINT ( 'NONE',  ( -83.32982269052723723, 31.07393428812022051, 35.00001200000000523 ) ) ;
#2450 = AXIS2_PLACEMENT_3D ( 'NONE', #7655, #13488, #9165 ) ;
#2451 = LINE ( 'NONE', #8237, #6914 ) ;
#2452 = VERTEX_POINT ( 'NONE', #114 ) ;
#2453 = LINE ( 'NONE', #1058, #9909 ) ;
#2454 = DIRECTION ( 'NONE',  ( -0.9876526153536341335, -0.1566598588826327021, 0.000000000000000000 ) ) ;
#2455 = VERTEX_POINT ( 'NONE', #3307 ) ;
#2456 = CIRCLE ( 'NONE', #7317, 1.500000000000000888 ) ;
#2457 = DIRECTION ( 'NONE',  ( -0.1566598588826321747, 0.9876526153536343555, 0.000000000000000000 ) ) ;
#2458 = EDGE_CURVE ( 'NONE', #15004, #2601, #993, .T. ) ;
#2459 = CARTESIAN_POINT ( 'NONE',  ( -24.31886431249228409, -24.10720463817513703, 21.65063509461101887 ) ) ;
#2460 = ORIENTED_EDGE ( 'NONE', *, *, #9208, .T. ) ;
#2461 = AXIS2_PLACEMENT_3D ( 'NONE', #7999, #14263, #12824 ) ;
#2462 = EDGE_CURVE ( 'NONE', #8941, #8532, #71, .T. ) ;
#2463 = DIRECTION ( 'NONE',  ( 0.000000000000000000, 0.000000000000000000, 1.000000000000000000 ) ) ;
#2464 = CARTESIAN_POINT ( 'NONE',  ( -67.07739975943471222, -25.82698556391886058, 8.660254037844417496 ) ) ;
#2465 = CARTESIAN_POINT ( 'NONE',  ( -79.48103206242137730, 1.792378103397237687, -3.092380961970916609 ) ) ;
#2466 = FACE_OUTER_BOUND ( 'NONE', #6512, .T. ) ;
#2467 = DIRECTION ( 'NONE',  ( -0.1566598588826321192, 0.9876526153536342445, 7.798540720466730171E-17 ) ) ;
#2468 = DIRECTION ( 'NONE',  ( -0.9876526153536336894, -0.1566598588826349503, 0.000000000000000000 ) ) ;
#2469 = VERTEX_POINT ( 'NONE', #6089 ) ;
#2470 = CARTESIAN_POINT ( 'NONE',  ( -126.5450966053943631, 9.599007176297428501, -2.520603730400377440 ) ) ;
#2471 = DIRECTION ( 'NONE',  ( 0.000000000000000000, 0.000000000000000000, -1.000000000000000000 ) ) ;
#2472 = AXIS2_PLACEMENT_3D ( 'NONE', #5439, #3997, #13856 ) ;
#2473 = CARTESIAN_POINT ( 'NONE',  ( 3.231158466157545206, -19.73726462726228092, 25.00000000000000711 ) ) ;
#2474 = AXIS2_PLACEMENT_3D ( 'NONE', #2902, #12776, #7301 ) ;
#2475 = VECTOR ( 'NONE', #16615, 1000.000000000000000 ) ;
#2476 = VERTEX_POINT ( 'NONE', #17572 ) ;
#2477 = CARTESIAN_POINT ( 'NONE',  ( -89.99999999999998579, -35.00000000000001421, 2.500000000000030198 ) ) ;
#2478 = ORIENTED_EDGE ( 'NONE', *, *, #13227, .F. ) ;
#2479 = ORIENTED_EDGE ( 'NONE', *, *, #7099, .T. ) ;
#2480 = MANIFOLD_SOLID_BREP ( 'Cavity1', #10549 ) ;
#2481 = FACE_BOUND ( 'NONE', #6430, .T. ) ;
#2482 = AXIS2_PLACEMENT_3D ( 'NONE', #16984, #11258, #2640 ) ;
#2483 = FACE_BOUND ( 'NONE', #9992, .T. ) ;
#2484 = VECTOR ( 'NONE', #16297, 1000.000000000000000 ) ;
#2485 = LINE ( 'NONE', #15360, #17967 ) ;
#2486 = ORIENTED_EDGE ( 'NONE', *, *, #10798, .F. ) ;
#2487 = ADVANCED_FACE ( 'NONE', ( #1812 ), #4558, .T. ) ;
#2488 = AXIS2_PLACEMENT_3D ( 'NONE', #10977, #1992, #13720 ) ;
#2489 = EDGE_CURVE ( 'NONE', #6795, #5802, #5832, .T. ) ;
#2490 = CARTESIAN_POINT ( 'NONE',  ( -71.02801022084922522, -26.45362499944938151, 4.330127018922218518 ) ) ;
#2491 = LINE ( 'NONE', #3699, #13363 ) ;
#2492 = AXIS2_PLACEMENT_3D ( 'NONE', #2054, #6442, #651 ) ;
#2493 = LINE ( 'NONE', #6858, #4409 ) ;
#2494 = EDGE_CURVE ( 'NONE', #10067, #10091, #380, .T. ) ;
#2495 = FACE_OUTER_BOUND ( 'NONE', #10053, .T. ) ;
#2496 = CARTESIAN_POINT ( 'NONE',  ( -20.86208015875457988, -23.55889513208593655, -12.99038105676658006 ) ) ;
#2497 = CARTESIAN_POINT ( 'NONE',  ( -62.63296299034337977, -25.12201619894701565, 12.99038105676661736 ) ) ;
#2498 = DIRECTION ( 'NONE',  ( -0.1566598588826321747, 0.9876526153536343555, 0.000000000000000000 ) ) ;
#2499 = FACE_OUTER_BOUND ( 'NONE', #7986, .T. ) ;
#2500 = CARTESIAN_POINT ( 'NONE',  ( 10.28861223506262412, -76.32329101363113466, 9.043241838514131834E-15 ) ) ;
#2501 = ORIENTED_EDGE ( 'NONE', *, *, #2145, .T. ) ;
#2502 = EDGE_LOOP ( 'NONE', ( #15673, #8880, #4795, #16546, #6404 ) ) ;
#2503 = LINE ( 'NONE', #9603, #6718 ) ;
#2504 = ORIENTED_EDGE ( 'NONE', *, *, #16437, .T. ) ;
#2505 = FACE_OUTER_BOUND ( 'NONE', #7205, .T. ) ;
#2506 = EDGE_LOOP ( 'NONE', ( #4361, #9243 ) ) ;
#2507 = CIRCLE ( 'NONE', #8266, 1.499999999999999556 ) ;
#2508 = CARTESIAN_POINT ( 'NONE',  ( -71.81027153490798298, 45.77027871590120611, 3.518396351564663682 ) ) ;
#2509 = DIRECTION ( 'NONE',  ( -0.9876526153536336894, -0.1566598588826349503, 0.000000000000000000 ) ) ;
#2510 = EDGE_CURVE ( 'NONE', #1139, #18416, #8247, .T. ) ;
#2511 = DIRECTION ( 'NONE',  ( -0.9876526153536336894, -0.1566598588826349503, 0.000000000000000000 ) ) ;
#2512 = CARTESIAN_POINT ( 'NONE',  ( -131.1055737289773617, -2.850701963179328668, -15.78184964806336055 ) ) ;
#2513 = DIRECTION ( 'NONE',  ( -0.9876526153536344665, -0.1566598588826304539, 0.000000000000000000 ) ) ;
#2514 = FACE_BOUND ( 'NONE', #2700, .T. ) ;
#2515 = ORIENTED_EDGE ( 'NONE', *, *, #12515, .T. ) ;
#2516 = ORIENTED_EDGE ( 'NONE', *, *, #15678, .F. ) ;
#2517 = CIRCLE ( 'NONE', #18298, 1.500000000000000888 ) ;
#2518 = FACE_BOUND ( 'NONE', #2760, .T. ) ;
#2519 = DIRECTION ( 'NONE',  ( -0.1566598588826321192, 0.9876526153536342445, 7.798540720466731404E-17 ) ) ;
#2520 = ORIENTED_EDGE ( 'NONE', *, *, #12264, .F. ) ;
#2521 = EDGE_CURVE ( 'NONE', #11293, #12109, #8557, .T. ) ;
#2522 = EDGE_LOOP ( 'NONE', ( #6844, #9418, #6094, #18318 ) ) ;
#2523 = EDGE_LOOP ( 'NONE', ( #13795, #17664 ) ) ;
#2524 = LINE ( 'NONE', #1123, #10007 ) ;
#2525 = CARTESIAN_POINT ( 'NONE',  ( 5.350349158294472218, -77.10659030804430358, -17.32050807568878525 ) ) ;
#2526 = DIRECTION ( 'NONE',  ( -0.1566598588826321192, 0.9876526153536342445, 7.798540720466731404E-17 ) ) ;
#2527 = DIRECTION ( 'NONE',  ( 0.000000000000000000, 0.000000000000000000, 1.000000000000000000 ) ) ;
#2528 = VECTOR ( 'NONE', #7212, 1000.000000000000000 ) ;
#2529 = DIRECTION ( 'NONE',  ( -0.9876526153536341335, -0.1566598588826327021, 0.000000000000000000 ) ) ;
#2530 = CARTESIAN_POINT ( 'NONE',  ( -167.4745151998187680, 32.15905408292206147, -2.500000000000000000 ) ) ;
#2531 = SHAPE_REPRESENTATION_RELATIONSHIP ( 'NONE' , 'NONE' ,  #17876, #16831 ) ;
#2532 = EDGE_CURVE ( 'NONE', #15648, #13882, #3979, .T. ) ;
#2533 = DIRECTION ( 'NONE',  ( -1.000000000000000000, 0.000000000000000000, 0.000000000000000000 ) ) ;
#2534 = EDGE_LOOP ( 'NONE', ( #16425, #7412 ) ) ;
#2535 = DIRECTION ( 'NONE',  ( -0.1566598588826321192, 0.9876526153536342445, 7.798540720466731404E-17 ) ) ;
#2536 = DIRECTION ( 'NONE',  ( -8.693966348389027220E-17, 1.991237296706375196E-16, -1.000000000000000000 ) ) ;
#2537 = VERTEX_POINT ( 'NONE', #10885 ) ;
#2538 = ORIENTED_EDGE ( 'NONE', *, *, #5486, .T. ) ;
#2539 = CARTESIAN_POINT ( 'NONE',  ( -77.44775222064782838, -27.47191408218647979, -12.99038105676658006 ) ) ;
#2540 = EDGE_CURVE ( 'NONE', #3070, #17772, #13819, .T. ) ;
#2541 = DIRECTION ( 'NONE',  ( -0.9876526153536341335, -0.1566598588826327021, 0.000000000000000000 ) ) ;
#2542 = ORIENTED_EDGE ( 'NONE', *, *, #7949, .T. ) ;
#2543 = ADVANCED_FACE ( 'NONE', ( #10779 ), #15168, .F. ) ;
#2544 = FACE_OUTER_BOUND ( 'NONE', #15336, .T. ) ;
#2545 = VERTEX_POINT ( 'NONE', #17850 ) ;
#2546 = DIRECTION ( 'NONE',  ( 0.000000000000000000, 0.000000000000000000, -1.000000000000000000 ) ) ;
#2547 = ORIENTED_EDGE ( 'NONE', *, *, #7098, .F. ) ;
#2548 = DIRECTION ( 'NONE',  ( 0.000000000000000000, 0.000000000000000000, 1.000000000000000000 ) ) ;
#2549 = LINE ( 'NONE', #14757, #636 ) ;
#2550 = CYLINDRICAL_SURFACE ( 'NONE', #10032, 1.500000000000001554 ) ;
#2551 = DIRECTION ( 'NONE',  ( -0.1566598588826321192, 0.9876526153536342445, 7.798540720466731404E-17 ) ) ;
#2552 = EDGE_CURVE ( 'NONE', #10229, #10439, #2183, .T. ) ;
#2553 = DIRECTION ( 'NONE',  ( -0.9876526153536341335, -0.1566598588826327021, 0.000000000000000000 ) ) ;
#2554 = CARTESIAN_POINT ( 'NONE',  ( 55.85952145814821534, 6.938893903907228378E-15, 35.00000000000000000 ) ) ;
#2555 = EDGE_CURVE ( 'NONE', #7813, #5152, #10948, .T. ) ;
#2556 = EDGE_CURVE ( 'NONE', #139, #7759, #11252, .T. ) ;
#2557 = CYLINDRICAL_SURFACE ( 'NONE', #16277, 2.200000000000000622 ) ;
#2558 = CARTESIAN_POINT ( 'NONE',  ( -43.08426400421124924, -27.08374195694514341, 17.32050807568881723 ) ) ;
#2559 = EDGE_CURVE ( 'NONE', #7022, #13460, #2801, .T. ) ;
#2560 = VERTEX_POINT ( 'NONE', #5001 ) ;
#2561 = VERTEX_POINT ( 'NONE', #9480 ) ;
#2562 = CARTESIAN_POINT ( 'NONE',  ( -88.82622559915370175, -29.27674910825304622, -24.99999999999999645 ) ) ;
#2563 = ORIENTED_EDGE ( 'NONE', *, *, #9742, .T. ) ;
#2564 = ORIENTED_EDGE ( 'NONE', *, *, #7249, .F. ) ;
#2565 = CARTESIAN_POINT ( 'NONE',  ( -52.96079015774756726, -28.65034054577146705, -17.32050807568878170 ) ) ;
#2566 = FACE_BOUND ( 'NONE', #17922, .T. ) ;
#2567 = CARTESIAN_POINT ( 'NONE',  ( -10.45209268736360997, -79.61314805016641571, 12.99038105676661203 ) ) ;
#2568 = CIRCLE ( 'NONE', #13150, 1.500000000000000888 ) ;
#2569 = ORIENTED_EDGE ( 'NONE', *, *, #11692, .F. ) ;
#2570 = CARTESIAN_POINT ( 'NONE',  ( -30.04042668367358360, -19.95224085582017182, 4.330127018922218518 ) ) ;
#2571 = CARTESIAN_POINT ( 'NONE',  ( -45.51376053241748565, -85.17457304049985112, 8.660254037844412167 ) ) ;
#2572 = ORIENTED_EDGE ( 'NONE', *, *, #16811, .F. ) ;
#2573 = ORIENTED_EDGE ( 'NONE', *, *, #17229, .T. ) ;
#2574 = ADVANCED_FACE ( 'NONE', ( #8157 ), #8849, .T. ) ;
#2575 = ORIENTED_EDGE ( 'NONE', *, *, #4514, .T. ) ;
#2576 = DIRECTION ( 'NONE',  ( 0.000000000000000000, 0.000000000000000000, 1.000000000000000000 ) ) ;
#2577 = FACE_OUTER_BOUND ( 'NONE', #5940, .T. ) ;
#2578 = DIRECTION ( 'NONE',  ( -0.9868632313631133801, 0.1615579233078772436, -0.000000000000000000 ) ) ;
#2579 = CARTESIAN_POINT ( 'NONE',  ( -14.44233815895597672, -22.54060604934882051, 21.65063509461101177 ) ) ;
#2580 = DIRECTION ( 'NONE',  ( -0.1566598588826321747, 0.9876526153536343555, 0.000000000000000000 ) ) ;
#2581 = VERTEX_POINT ( 'NONE', #18140 ) ;
#2582 = EDGE_CURVE ( 'NONE', #7610, #13224, #5110, .T. ) ;
#2583 = VERTEX_POINT ( 'NONE', #3768 ) ;
#2584 = ORIENTED_EDGE ( 'NONE', *, *, #5946, .F. ) ;
#2585 = CARTESIAN_POINT ( 'NONE',  ( -70.20507591625822386, -89.09106951256565310, 8.660254037844412167 ) ) ;
#2586 = ADVANCED_FACE ( 'NONE', ( #7778 ), #10054, .T. ) ;
#2587 = EDGE_LOOP ( 'NONE', ( #16141, #7529, #1388, #12352 ) ) ;
#2588 = DIRECTION ( 'NONE',  ( -0.1566598588826321192, 0.9876526153536342445, 7.798540720466730171E-17 ) ) ;
#2589 = CARTESIAN_POINT ( 'NONE',  ( -67.57122606711153878, -25.90531549336016326, -12.99038105676658006 ) ) ;
#2590 = PRODUCT ( 'Heavy-Duty Perforated Sieve Plate', 'Heavy-Duty Perforated Sieve Plate', '', ( #6883 ) ) ;
#2591 = MANIFOLD_SOLID_BREP ( 'Boss-Extrude3', #16010 ) ;
#2592 = CARTESIAN_POINT ( 'NONE',  ( -77.44775222064782838, -27.47191408218648689, 4.330127018922218518 ) ) ;
#2593 = UNCERTAINTY_MEASURE_WITH_UNIT (LENGTH_MEASURE( 1.000000000000000082E-05 ), #7823, 'distance_accuracy_value', 'NONE');
#2594 = VECTOR ( 'NONE', #13746, 1000.000000000000000 ) ;
#2595 = CARTESIAN_POINT ( 'NONE',  ( -70.03008040050728766, 45.01279934630233015, 6.841710791646147705 ) ) ;
#2596 = CONTEXT_DEPENDENT_SHAPE_REPRESENTATION ( #5316, #11357 ) ;
#2597 = CARTESIAN_POINT ( 'NONE',  ( 0.000000000000000000, 0.000000000000000000, -19.99999999999999645 ) ) ;
#2598 = DIRECTION ( 'NONE',  ( -0.9876526153536344665, -0.1566598588826304539, 0.000000000000000000 ) ) ;
#2599 = DIRECTION ( 'NONE',  ( -0.1566598588826321747, 0.9876526153536343555, 0.000000000000000000 ) ) ;
#2600 = DIRECTION ( 'NONE',  ( -0.1566598588826321192, 0.9876526153536342445, 7.798540720466731404E-17 ) ) ;
#2601 = VERTEX_POINT ( 'NONE', #6748 ) ;
#2602 = ORIENTED_EDGE ( 'NONE', *, *, #7468, .T. ) ;
#2603 = DIRECTION ( 'NONE',  ( -0.1566598588826321747, 0.9876526153536343555, 0.000000000000000000 ) ) ;
#2604 = LINE ( 'NONE', #4012, #7607 ) ;
#2605 = AXIS2_PLACEMENT_3D ( 'NONE', #10255, #13184, #5234 ) ;
#2606 = EDGE_LOOP ( 'NONE', ( #4453, #290, #8768, #8101, #18259, #11902, #6738, #11595, #18767 ) ) ;
#2607 = EDGE_CURVE ( 'NONE', #6427, #15608, #6736, .T. ) ;
#2608 = AXIS2_PLACEMENT_3D ( 'NONE', #4351, #18716, #16004 ) ;
#2609 = ORIENTED_EDGE ( 'NONE', *, *, #9681, .F. ) ;
#2610 = DIRECTION ( 'NONE',  ( 1.000000000000000000, 0.000000000000000000, 0.000000000000000000 ) ) ;
#2611 = EDGE_CURVE ( 'NONE', #5881, #15709, #11554, .T. ) ;
#2612 = DIRECTION ( 'NONE',  ( -0.1566598588826321192, 0.9876526153536342445, 7.798540720466730171E-17 ) ) ;
#2613 = CARTESIAN_POINT ( 'NONE',  ( -59.67000514428248437, -24.65203662229911785, -4.330127018922180326 ) ) ;
#2614 = EDGE_LOOP ( 'NONE', ( #11880, #14288 ) ) ;
#2615 = CARTESIAN_POINT ( 'NONE',  ( -44.03228160938702018, -84.93958325217590755, 17.32050807568881368 ) ) ;
#2616 = VECTOR ( 'NONE', #2844, 1000.000000000000000 ) ;
#2617 = DIRECTION ( 'NONE',  ( -0.000000000000000000, -0.000000000000000000, -1.000000000000000000 ) ) ;
#2618 = DIRECTION ( 'NONE',  ( -0.1566598588826321747, 0.9876526153536343555, 0.000000000000000000 ) ) ;
#2619 = CARTESIAN_POINT ( 'NONE',  ( -3.578159390066044665, -20.81734760163988440, -8.660254037844383745 ) ) ;
#2620 = AXIS2_PLACEMENT_3D ( 'NONE', #7373, #18779, #13126 ) ;
#2621 = DIRECTION ( 'NONE',  ( -0.9876526153536336894, -0.1566598588826349503, 0.000000000000000000 ) ) ;
#2622 = DIRECTION ( 'NONE',  ( -1.000000000000000000, 0.000000000000000000, 0.000000000000000000 ) ) ;
#2623 = LINE ( 'NONE', #15323, #15956 ) ;
#2624 = ORIENTED_EDGE ( 'NONE', *, *, #1733, .F. ) ;
#2625 = DIRECTION ( 'NONE',  ( -0.1566598588826326743, -0.9876526153536341335, 0.000000000000000000 ) ) ;
#2626 = CARTESIAN_POINT ( 'NONE',  ( -76.94165664733894516, -1.794943808410583763, 6.745229976240270098 ) ) ;
#2627 = ORIENTED_EDGE ( 'NONE', *, *, #7093, .F. ) ;
#2628 = CIRCLE ( 'NONE', #9279, 1.500000000000001332 ) ;
#2629 = VECTOR ( 'NONE', #6174, 1000.000000000000000 ) ;
#2630 = DIRECTION ( 'NONE',  ( -0.1566598588826321747, 0.9876526153536343555, 0.000000000000000000 ) ) ;
#2631 = EDGE_LOOP ( 'NONE', ( #14433, #10981 ) ) ;
#2632 = ORIENTED_EDGE ( 'NONE', *, *, #5302, .F. ) ;
#2633 = EDGE_CURVE ( 'NONE', #7092, #13293, #3379, .T. ) ;
#2634 = CIRCLE ( 'NONE', #14437, 1.500000000000001332 ) ;
#2635 = LINE ( 'NONE', #18792, #6423 ) ;
#2636 = CIRCLE ( 'NONE', #6587, 1.500000000000000000 ) ;
#2637 = DIRECTION ( 'NONE',  ( -0.000000000000000000, -0.000000000000000000, -1.000000000000000000 ) ) ;
#2638 = FACE_OUTER_BOUND ( 'NONE', #10893, .T. ) ;
#2639 = ORIENTED_EDGE ( 'NONE', *, *, #6124, .F. ) ;
#2640 = DIRECTION ( 'NONE',  ( 0.000000000000000000, 0.000000000000000000, 1.000000000000000000 ) ) ;
#2641 = FACE_OUTER_BOUND ( 'NONE', #10045, .T. ) ;
#2642 = ADVANCED_FACE ( 'NONE', ( #3965 ), #4259, .F. ) ;
#2643 = VECTOR ( 'NONE', #8593, 1000.000000000000000 ) ;
#2644 = DIRECTION ( 'NONE',  ( -0.1566598588826321192, 0.9876526153536342445, 7.798540720466731404E-17 ) ) ;
#2645 = CYLINDRICAL_SURFACE ( 'NONE', #6979, 1.500000000000000888 ) ;
#2646 = DIRECTION ( 'NONE',  ( -0.1566598588826321747, 0.9876526153536343555, 0.000000000000000000 ) ) ;
#2647 = DIRECTION ( 'NONE',  ( -1.000000000000000000, 0.000000000000000000, 0.000000000000000000 ) ) ;
#2648 = CARTESIAN_POINT ( 'NONE',  ( -31.68662391746665463, -82.98133501614300656, 4.330127018922213189 ) ) ;
#2649 = CARTESIAN_POINT ( 'NONE',  ( -71.02801022084922522, -26.45362499944937795, -4.330127018922180326 ) ) ;
#2650 = MECHANICAL_DESIGN_GEOMETRIC_PRESENTATION_REPRESENTATION (  '', ( #3830 ), #534 ) ;
#2651 = ORIENTED_EDGE ( 'NONE', *, *, #3022, .F. ) ;
#2652 = CIRCLE ( 'NONE', #14753, 1.500000000000000888 ) ;
#2653 = ORIENTED_EDGE ( 'NONE', *, *, #14593, .T. ) ;
#2654 = VERTEX_POINT ( 'NONE', #9678 ) ;
#2655 = DIRECTION ( 'NONE',  ( -0.9876526153536336894, -0.1566598588826349503, 0.000000000000000000 ) ) ;
#2656 = ORIENTED_EDGE ( 'NONE', *, *, #11281, .F. ) ;
#2657 = ORIENTED_EDGE ( 'NONE', *, *, #10702, .T. ) ;
#2658 = DIRECTION ( 'NONE',  ( 0.000000000000000000, 0.000000000000000000, 1.000000000000000000 ) ) ;
#2659 = FACE_BOUND ( 'NONE', #9383, .T. ) ;
#2660 = EDGE_CURVE ( 'NONE', #18388, #3138, #17169, .T. ) ;
#2661 = ADVANCED_FACE ( 'NONE', ( #1072 ), #15540, .F. ) ;
#2662 = CARTESIAN_POINT ( 'NONE',  ( -44.07191661956488105, -27.24040181582776299, -12.99038105676658006 ) ) ;
#2663 = ORIENTED_EDGE ( 'NONE', *, *, #18603, .F. ) ;
#2664 = AXIS2_PLACEMENT_3D ( 'NONE', #4048, #15343, #8340 ) ;
#2665 = ADVANCED_FACE ( 'NONE', ( #4151 ), #9855, .F. ) ;
#2666 = DIRECTION ( 'NONE',  ( -0.1566598588826321192, 0.9876526153536342445, 7.798540720466730171E-17 ) ) ;
#2667 = EDGE_CURVE ( 'NONE', #12027, #13473, #9158, .T. ) ;
#2668 = ORIENTED_EDGE ( 'NONE', *, *, #15638, .T. ) ;
#2669 = AXIS2_PLACEMENT_3D ( 'NONE', #7851, #14950, #12083 ) ;
#2670 = CARTESIAN_POINT ( 'NONE',  ( -40.41077914488671041, -21.59716937408779458, -8.660254037844380193 ) ) ;
#2671 = DIRECTION ( 'NONE',  ( 0.000000000000000000, -1.000000000000000000, 0.000000000000000000 ) ) ;
#2672 = AXIS2_PLACEMENT_3D ( 'NONE', #15675, #5922, #2702 ) ;
#2673 = CARTESIAN_POINT ( 'NONE',  ( -55.42992169613162190, -29.04199019297804085, 12.99038105676661736 ) ) ;
#2674 = ORIENTED_EDGE ( 'NONE', *, *, #14267, .F. ) ;
#2675 = AXIS2_PLACEMENT_3D ( 'NONE', #1611, #5594, #13142 ) ;
#2676 = ORIENTED_EDGE ( 'NONE', *, *, #16258, .F. ) ;
#2677 = EDGE_LOOP ( 'NONE', ( #5363, #7131 ) ) ;
#2678 = DIRECTION ( 'NONE',  ( -0.1566598588826321747, 0.9876526153536343555, 0.000000000000000000 ) ) ;
#2679 = ORIENTED_EDGE ( 'NONE', *, *, #1905, .F. ) ;
#2680 = EDGE_LOOP ( 'NONE', ( #18041, #3184, #7910, #2999 ) ) ;
#2681 = VERTEX_POINT ( 'NONE', #14111 ) ;
#2682 = CARTESIAN_POINT ( 'NONE',  ( 2.000000000000000000, 2.449293598294706414E-16, 24.99999999999999289 ) ) ;
#2683 = AXIS2_PLACEMENT_3D ( 'NONE', #14973, #16306, #14611 ) ;
#2684 = CYLINDRICAL_SURFACE ( 'NONE', #16025, 144.0000000000000284 ) ;
#2685 = ADVANCED_FACE ( 'NONE', ( #12676 ), #5407, .F. ) ;
#2686 = VECTOR ( 'NONE', #8972, 1000.000000000000000 ) ;
#2687 = ADVANCED_FACE ( 'NONE', ( #15728 ), #2557, .F. ) ;
#2688 = VECTOR ( 'NONE', #18062, 1000.000000000000000 ) ;
#2689 = PRODUCT_RELATED_PRODUCT_CATEGORY ( 'part', '', ( #15287 ) ) ;
#2690 = CARTESIAN_POINT ( 'NONE',  ( -24.81269062016911064, -24.18553456761645393, -8.660254037844380193 ) ) ;
#2691 = ADVANCED_FACE ( 'NONE', ( #17279, #6940, #5509 ), #1344, .F. ) ;
#2692 = VERTEX_POINT ( 'NONE', #8439 ) ;
#2693 = DIRECTION ( 'NONE',  ( -0.1566598588826321192, 0.9876526153536342445, 7.798540720466731404E-17 ) ) ;
#2694 = DIRECTION ( 'NONE',  ( -0.9876526153536344665, -0.1566598588826304539, 0.000000000000000000 ) ) ;
#2695 = VERTEX_POINT ( 'NONE', #10123 ) ;
#2696 = DIRECTION ( 'NONE',  ( -0.1566598588826321747, 0.9876526153536343555, 0.000000000000000000 ) ) ;
#2697 = VECTOR ( 'NONE', #11946, 1000.000000000000000 ) ;
#2698 = CARTESIAN_POINT ( 'NONE',  ( -34.19539046602857724, -25.67380322700145356, -4.330127018922181215 ) ) ;
#2699 = VERTEX_POINT ( 'NONE', #1784 ) ;
#2700 = EDGE_LOOP ( 'NONE', ( #3536, #4135 ) ) ;
#2701 = CARTESIAN_POINT ( 'NONE',  ( -43.86756329862441817, -22.14547888017700572, -8.660254037844380193 ) ) ;
#2702 = DIRECTION ( 'NONE',  ( -0.9876526153536336894, -0.1566598588826349503, 0.000000000000000000 ) ) ;
#2703 = CIRCLE ( 'NONE', #13278, 1.500000000000000888 ) ;
#2704 = LINE ( 'NONE', #16071, #12408 ) ;
#2705 = VECTOR ( 'NONE', #15391, 1000.000000000000000 ) ;
#2706 = VECTOR ( 'NONE', #9460, 1000.000000000000000 ) ;
#2707 = AXIS2_PLACEMENT_3D ( 'NONE', #1942, #12050, #17710 ) ;
#2708 = EDGE_LOOP ( 'NONE', ( #1911, #14500, #1537, #1738 ) ) ;
#2709 = LINE ( 'NONE', #6716, #12422 ) ;
#2710 = CARTESIAN_POINT ( 'NONE',  ( -16.70711637639958269, -17.83733276090463704, -4.330127018922180326 ) ) ;
#2711 = VECTOR ( 'NONE', #4016, 1000.000000000000000 ) ;
#2713 = CARTESIAN_POINT ( 'NONE',  ( -128.1677737538112751, 9.451028958170518024, 3.279750847804448366 ) ) ;
#2712 = AXIS2_PLACEMENT_3D ( 'NONE', #18399, #18501, #9904 ) ;
#2714 = FACE_OUTER_BOUND ( 'NONE', #8482, .T. ) ;
#2715 = CYLINDRICAL_SURFACE ( 'NONE', #5709, 2.500000000000002220 ) ;
#2716 = EDGE_CURVE ( 'NONE', #1265, #2879, #5705, .T. ) ;
#2717 = ORIENTED_EDGE ( 'NONE', *, *, #13276, .T. ) ;
#2718 = AXIS2_PLACEMENT_3D ( 'NONE', #435, #345, #9052 ) ;
#2719 = ADVANCED_FACE ( 'NONE', ( #10488 ), #5959, .F. ) ;
#2720 = CARTESIAN_POINT ( 'NONE',  ( -309.1404785418517918, -2.850701963179328668, 9.951701414186818625E-16 ) ) ;
#2721 = CIRCLE ( 'NONE', #13301, 1.500000000000000000 ) ;
#2722 = CARTESIAN_POINT ( 'NONE',  ( -59.38053215754615621, -29.66862962850855112, 17.32050807568881723 ) ) ;
#2723 = DIRECTION ( 'NONE',  ( 1.000000000000000000, 0.000000000000000000, 0.000000000000000000 ) ) ;
#2724 = CARTESIAN_POINT ( 'NONE',  ( -42.87991068327077926, -21.98881902129437904, 4.330127018922218518 ) ) ;
#2725 = ORIENTED_EDGE ( 'NONE', *, *, #4906, .F. ) ;
#2726 = LINE ( 'NONE', #4126, #10310 ) ;
#2727 = EDGE_CURVE ( 'NONE', #4996, #6863, #17526, .T. ) ;
#2729 = ORIENTED_EDGE ( 'NONE', *, *, #9852, .T. ) ;
#2728 = DIRECTION ( 'NONE',  ( -0.1566598588826321192, 0.9876526153536342445, 7.798540720466731404E-17 ) ) ;
#2730 = AXIS2_PLACEMENT_3D ( 'NONE', #1963, #2055, #2509 ) ;
#2731 = B_SPLINE_CURVE_WITH_KNOTS ( 'NONE', 3,
 ( #15742, #17379, #4363, #12879 ),
 .UNSPECIFIED., .F., .F.,
 ( 4, 4 ),
 ( 0.000000000000000000, 0.003000475340473851647 ),
 .UNSPECIFIED. ) ;
#2732 = VERTEX_POINT ( 'NONE', #7313 ) ;
#2733 = CARTESIAN_POINT ( 'NONE',  ( -66.25446545484369665, -88.46443007703511796, 12.99038105676661203 ) ) ;
#2734 = DIRECTION ( 'NONE',  ( -0.9876526153536341335, -0.1566598588826327021, 0.000000000000000000 ) ) ;
#2735 = CIRCLE ( 'NONE', #3320, 1.500000000000001332 ) ;
#2736 = ORIENTED_EDGE ( 'NONE', *, *, #11008, .F. ) ;
#2737 = ORIENTED_EDGE ( 'NONE', *, *, #4285, .T. ) ;
#2738 = AXIS2_PLACEMENT_3D ( 'NONE', #17596, #4579, #8487 ) ;
#2739 = CIRCLE ( 'NONE', #329, 1.500000000000000888 ) ;
#2740 = CARTESIAN_POINT ( 'NONE',  ( -168.4538323585589694, 31.95594125380575434, 2.500000000000000000 ) ) ;
#2741 = CARTESIAN_POINT ( 'NONE',  ( -85.86167379012967160, 34.32252072304513746, 35.00000000000000000 ) ) ;
#2742 = DIRECTION ( 'NONE',  ( 0.000000000000000000, 0.000000000000000000, 1.000000000000000000 ) ) ;
#2743 = CARTESIAN_POINT ( 'NONE',  ( -63.62061560569701157, -25.27867605782964588, 8.660254037844417496 ) ) ;
#2744 = PLANE ( 'NONE',  #4472 ) ;
#2745 = AXIS2_PLACEMENT_3D ( 'NONE', #9541, #3454, #13780 ) ;
#2746 = CARTESIAN_POINT ( 'NONE',  ( -57.89905323451569785, -29.43363984018461466, 8.660254037844417496 ) ) ;
#2747 = CYLINDRICAL_SURFACE ( 'NONE', #1579, 1.500000000000001554 ) ;
#2748 = VECTOR ( 'NONE', #8691, 1000.000000000000000 ) ;
#2749 = DIRECTION ( 'NONE',  ( -0.9876526153536336894, -0.1566598588826349503, 0.000000000000000000 ) ) ;
#2750 = DIRECTION ( 'NONE',  ( -0.1566598588826321747, 0.9876526153536343555, 0.000000000000000000 ) ) ;
#2751 = CARTESIAN_POINT ( 'NONE',  ( -52.75643683680708307, -23.55541761012069557, 4.330127018922218518 ) ) ;
#2752 = EDGE_CURVE ( 'NONE', #4620, #17453, #3853, .T. ) ;
#2753 = CARTESIAN_POINT ( 'NONE',  ( -1.892327146095121204, -15.48743487766515337, -4.330127018922183879 ) ) ;
#2754 = CIRCLE ( 'NONE', #16365, 1.500000000000000888 ) ;
#2755 = DIRECTION ( 'NONE',  ( 0.000000000000000000, 0.000000000000000000, 1.000000000000000000 ) ) ;
#2756 = VERTEX_POINT ( 'NONE', #265 ) ;
#2757 = AXIS2_PLACEMENT_3D ( 'NONE', #17132, #8113, #18209 ) ;
#2758 = ORIENTED_EDGE ( 'NONE', *, *, #9726, .T. ) ;
#2759 = DIRECTION ( 'NONE',  ( -0.1566598588826321192, 0.9876526153536342445, 7.798540720466730171E-17 ) ) ;
#2760 = EDGE_LOOP ( 'NONE', ( #6345, #14303 ) ) ;
#2761 = EDGE_CURVE ( 'NONE', #16216, #4058, #15070, .T. ) ;
#2762 = ORIENTED_EDGE ( 'NONE', *, *, #3409, .T. ) ;
#2763 = VECTOR ( 'NONE', #3525, 1000.000000000000114 ) ;
#2764 = EDGE_LOOP ( 'NONE', ( #5604, #4078, #18302, #15584 ) ) ;
#2765 = CARTESIAN_POINT ( 'NONE',  ( -59.67000514428248437, -24.65203662229911075, -21.65063509461098334 ) ) ;
#2766 = EDGE_CURVE ( 'NONE', #14892, #18229, #250, .T. ) ;
#2767 = AXIS2_PLACEMENT_3D ( 'NONE', #16850, #12543, #14067 ) ;
#2768 = FACE_BOUND ( 'NONE', #962, .T. ) ;
#2769 = CIRCLE ( 'NONE', #4275, 1.500000000000000888 ) ;
#2770 = CARTESIAN_POINT ( 'NONE',  ( -77.50987606495345972, -0.1965428547086033040, -5.115516238835398966 ) ) ;
#2771 = CYLINDRICAL_SURFACE ( 'NONE', #4192, 1.500000000000001554 ) ;
#2772 = FACE_BOUND ( 'NONE', #16689, .T. ) ;
#2773 = VECTOR ( 'NONE', #4247, 1000.000000000000000 ) ;
#2774 = AXIS2_PLACEMENT_3D ( 'NONE', #5353, #15659, #4301 ) ;
#2775 = ORIENTED_EDGE ( 'NONE', *, *, #6196, .F. ) ;
#2776 = DIRECTION ( 'NONE',  ( -0.9876526153536336894, -0.1566598588826349503, 0.000000000000000000 ) ) ;
#2777 = CARTESIAN_POINT ( 'NONE',  ( 55.85952145814821534, 6.938893903907228378E-15, 30.00000000000000000 ) ) ;
#2778 = CARTESIAN_POINT ( 'NONE',  ( -129.1404785418517918, -2.850701963179326892, -12.74754878398196389 ) ) ;
#2779 = AXIS2_PLACEMENT_3D ( 'NONE', #14313, #5502, #12494 ) ;
#2780 = EDGE_CURVE ( 'NONE', #13776, #2561, #17653, .T. ) ;
#2781 = EDGE_LOOP ( 'NONE', ( #13137, #4159, #18241, #13078 ) ) ;
#2782 = EDGE_CURVE ( 'NONE', #16444, #8059, #4710, .T. ) ;
#2783 = CIRCLE ( 'NONE', #8239, 1.500000000000001332 ) ;
#2784 = ORIENTED_EDGE ( 'NONE', *, *, #14509, .T. ) ;
#2785 = ORIENTED_EDGE ( 'NONE', *, *, #543, .T. ) ;
#2786 = CARTESIAN_POINT ( 'NONE',  ( 1.893565004556770903, -77.65489981413351472, 8.660254037844408614 ) ) ;
#2787 = B_SPLINE_CURVE_WITH_KNOTS ( 'NONE', 3,
 ( #2389, #15281, #16923, #13956, #12524, #10912, #15377, #2295, #6578, #18367, #12327, #13849, #16736, #901, #12436, #5340 ),
 .UNSPECIFIED., .F., .F.,
 ( 4, 2, 2, 2, 2, 2, 2, 4 ),
 ( 1.734723475976807094E-18, 0.0006035471611761681829, 0.001207094322352334631, 0.001810641483528501296, 0.002414188644704666660, 0.003017735805880831807, 0.003621282967056997388, 0.004828377289409254390 ),
 .UNSPECIFIED. ) ;
#2788 = ORIENTED_EDGE ( 'NONE', *, *, #9097, .T. ) ;
#2789 = FACE_BOUND ( 'NONE', #10321, .T. ) ;
#2790 = VECTOR ( 'NONE', #18267, 1000.000000000000000 ) ;
#2791 = CYLINDRICAL_SURFACE ( 'NONE', #15414, 1.500000000000001554 ) ;
#2792 = ORIENTED_EDGE ( 'NONE', *, *, #3504, .F. ) ;
#2793 = FACE_OUTER_BOUND ( 'NONE', #14555, .T. ) ;
#2794 = CYLINDRICAL_SURFACE ( 'NONE', #1847, 1.500000000000001554 ) ;
#2795 = AXIS2_PLACEMENT_3D ( 'NONE', #13893, #2618, #8317 ) ;
#2796 = DIRECTION ( 'NONE',  ( -0.1566598588826321192, 0.9876526153536342445, 7.798540720466730171E-17 ) ) ;
#2797 = APPLICATION_PROTOCOL_DEFINITION ( 'draft international standard', 'automotive_design', 1998, #11355 ) ;
#2798 = CARTESIAN_POINT ( 'NONE',  ( -84.23462711737164454, 33.01666666666666572, 35.00000000000000000 ) ) ;
#2799 = CARTESIAN_POINT ( 'NONE',  ( -19.34096622554629263, -81.02308678011009135, -17.32050807568878525 ) ) ;
#2800 = ADVANCED_FACE ( 'NONE', ( #11893 ), #8713, .F. ) ;
#2801 = CIRCLE ( 'NONE', #2488, 1.499999999999999556 ) ;
#2802 = CARTESIAN_POINT ( 'NONE',  ( -33.20773785067495254, -25.51714336811882688, 1.869203119972154228E-14 ) ) ;
#2803 = EDGE_CURVE ( 'NONE', #10018, #2423, #14766, .T. ) ;
#2804 = EDGE_LOOP ( 'NONE', ( #13674, #17767 ) ) ;
#2805 = ORIENTED_EDGE ( 'NONE', *, *, #727, .F. ) ;
#2806 = LINE ( 'NONE', #12738, #16601 ) ;
#2807 = DIRECTION ( 'NONE',  ( -0.1566598588826321192, 0.9876526153536342445, 7.798540720466731404E-17 ) ) ;
#2808 = CARTESIAN_POINT ( 'NONE',  ( -11.97320662057189899, -22.14895640214223960, 17.32050807568881012 ) ) ;
#2809 = CIRCLE ( 'NONE', #9775, 1.500000000000000444 ) ;
#2810 = ORIENTED_EDGE ( 'NONE', *, *, #8805, .T. ) ;
#2811 = CARTESIAN_POINT ( 'NONE',  ( -36.46016868347219742, -20.97052993855726655, -21.65063509461097979 ) ) ;
#2812 = LINE ( 'NONE', #14077, #6084 ) ;
#2813 = DIRECTION ( 'NONE',  ( -0.1566598588826321192, 0.9876526153536342445, 7.798540720466730171E-17 ) ) ;
#2814 = DIRECTION ( 'NONE',  ( -0.1566598588826321747, 0.9876526153536343555, 0.000000000000000000 ) ) ;
#2815 = ORIENTED_EDGE ( 'NONE', *, *, #6698, .T. ) ;
#2816 = AXIS2_PLACEMENT_3D ( 'NONE', #2075, #13632, #18035 ) ;
#2817 = DIRECTION ( 'NONE',  ( -0.1566598588826321747, 0.9876526153536343555, 0.000000000000000000 ) ) ;
#2818 = DIRECTION ( 'NONE',  ( -0.1566598588826321192, 0.9876526153536342445, 7.798540720466730171E-17 ) ) ;
#2819 = CARTESIAN_POINT ( 'NONE',  ( -20.65772683781411345, -18.46397219643516507, 17.32050807568881012 ) ) ;
#2820 = DIRECTION ( 'NONE',  ( -0.1566598588826321192, 0.9876526153536342445, 7.798540720466730171E-17 ) ) ;
#2821 = ORIENTED_EDGE ( 'NONE', *, *, #1702, .F. ) ;
#2822 = DIRECTION ( 'NONE',  ( -0.9876526153536341335, -0.1566598588826327021, 0.000000000000000000 ) ) ;
#2823 = CARTESIAN_POINT ( 'NONE',  ( -40.41077914488671041, -21.59716937408780169, 8.660254037844417496 ) ) ;
#2824 = ORIENTED_EDGE ( 'NONE', *, *, #6269, .T. ) ;
#2825 = ORIENTED_EDGE ( 'NONE', *, *, #123, .T. ) ;
#2826 = CARTESIAN_POINT ( 'NONE',  ( -19.38060123572413218, -23.32390534376198232, 21.65063509461101177 ) ) ;
#2827 = ORIENTED_EDGE ( 'NONE', *, *, #2372, .T. ) ;
#2828 = EDGE_CURVE ( 'NONE', #626, #8310, #9321, .T. ) ;
#2829 = EDGE_CURVE ( 'NONE', #8415, #719, #4475, .T. ) ;
#2830 = EDGE_LOOP ( 'NONE', ( #2296, #12859, #3885, #737 ) ) ;
#2831 = CARTESIAN_POINT ( 'NONE',  ( -77.65210554158829837, -32.56683701783724416, -17.32050807568878170 ) ) ;
#2832 = DIRECTION ( 'NONE',  ( -0.1566598588826321192, 0.9876526153536342445, 7.798540720466731404E-17 ) ) ;
#2833 = DIRECTION ( 'NONE',  ( -0.1566598588826321192, 0.9876526153536342445, 7.798540720466730171E-17 ) ) ;
#2834 = CARTESIAN_POINT ( 'NONE',  ( -43.08426400421124924, -27.08374195694514341, 8.660254037844417496 ) ) ;
#2835 = DIRECTION ( 'NONE',  ( -0.1566598588826321192, 0.9876526153536342445, 7.798540720466730171E-17 ) ) ;
#2836 = DIRECTION ( 'NONE',  ( -0.1566598588826321192, 0.9876526153536342445, 7.798540720466731404E-17 ) ) ;
#2837 = LINE ( 'NONE', #10122, #18396 ) ;
#2838 = CIRCLE ( 'NONE', #8602, 1.500000000000000444 ) ;
#2839 = CARTESIAN_POINT ( 'NONE',  ( -35.14340807120434818, -83.52964452223221770, 21.65063509461101532 ) ) ;
#2840 = ORIENTED_EDGE ( 'NONE', *, *, #12389, .T. ) ;
#2841 = DIRECTION ( 'NONE',  ( -0.9876526153536341335, -0.1566598588826327021, 0.000000000000000000 ) ) ;
#2842 = ORIENTED_EDGE ( 'NONE', *, *, #15504, .F. ) ;
#2843 = EDGE_LOOP ( 'NONE', ( #15234, #11312, #5562, #5738 ) ) ;
#2844 = DIRECTION ( 'NONE',  ( -0.000000000000000000, -0.000000000000000000, -1.000000000000000000 ) ) ;
#2845 = ORIENTED_EDGE ( 'NONE', *, *, #17537, .F. ) ;
#2846 = CARTESIAN_POINT ( 'NONE',  ( -36.46016868347219742, -20.97052993855726655, -21.65063509461097979 ) ) ;
#2847 = EDGE_CURVE ( 'NONE', #3794, #16655, #1431, .T. ) ;
#2848 = DIRECTION ( 'NONE',  ( -0.1566598588826321192, 0.9876526153536342445, 7.798540720466730171E-17 ) ) ;
#2849 = ORIENTED_EDGE ( 'NONE', *, *, #304, .F. ) ;
#2850 = EDGE_CURVE ( 'NONE', #4660, #11687, #14171, .T. ) ;
#2851 = DIRECTION ( 'NONE',  ( -0.000000000000000000, -0.000000000000000000, -1.000000000000000000 ) ) ;
#2852 = DIRECTION ( 'NONE',  ( -0.9876526153536336894, -0.1566598588826350336, 0.000000000000000000 ) ) ;
#2853 = DIRECTION ( 'NONE',  ( -0.1856185419698762884, 0.9826218788918642533, 0.000000000000000000 ) ) ;
#2854 = FACE_BOUND ( 'NONE', #11269, .T. ) ;
#2855 = DIRECTION ( 'NONE',  ( -0.9876526153536344665, -0.1566598588826304539, 0.000000000000000000 ) ) ;
#2856 = ORIENTED_EDGE ( 'NONE', *, *, #12161, .T. ) ;
#2857 = ORIENTED_EDGE ( 'NONE', *, *, #10238, .F. ) ;
#2858 = ORIENTED_EDGE ( 'NONE', *, *, #18462, .F. ) ;
#2859 = DIRECTION ( 'NONE',  ( 1.000000000000000000, 0.000000000000000000, 0.000000000000000000 ) ) ;
#2860 = ORIENTED_EDGE ( 'NONE', *, *, #12840, .F. ) ;
#2861 = AXIS2_PLACEMENT_3D ( 'NONE', #15696, #2622, #10781 ) ;
#2862 = FACE_OUTER_BOUND ( 'NONE', #16925, .T. ) ;
#2863 = CARTESIAN_POINT ( 'NONE',  ( -62.13913668266656032, -25.04368626950570231, 8.660254037844417496 ) ) ;
#2864 = EDGE_CURVE ( 'NONE', #1556, #9635, #3017, .T. ) ;
#2865 = CARTESIAN_POINT ( 'NONE',  ( -129.1404785418517918, -2.850701963179326892, -12.74754878398196389 ) ) ;
#2866 = CARTESIAN_POINT ( 'NONE',  ( 0.5768043922889515285, -15.09578523045857601, -17.32050807568878170 ) ) ;
#2867 = ADVANCED_FACE ( 'NONE', ( #11536 ), #10216, .F. ) ;
#2868 = CARTESIAN_POINT ( 'NONE',  ( -172.8945038000772456, 56.46685571404672999, 2.584671478510881748 ) ) ;
#2869 = VECTOR ( 'NONE', #13484, 1000.000000000000000 ) ;
#2870 = EDGE_CURVE ( 'NONE', #610, #12140, #10520, .T. ) ;
#2871 = CARTESIAN_POINT ( 'NONE',  ( -129.1404785418517918, 9.649298036820672664, 2.500000000000000000 ) ) ;
#2872 = CARTESIAN_POINT ( 'NONE',  ( -70.03007184274690644, 45.01279570493660742, -6.843761338458851817 ) ) ;
#2873 = VERTEX_POINT ( 'NONE', #13147 ) ;
#2874 = ORIENTED_EDGE ( 'NONE', *, *, #14245, .F. ) ;
#2875 = CYLINDRICAL_SURFACE ( 'NONE', #2672, 1.500000000000001554 ) ;
#2876 = DIRECTION ( 'NONE',  ( -0.1566598588826321192, 0.9876526153536342445, 7.798540720466730171E-17 ) ) ;
#2877 = CYLINDRICAL_SURFACE ( 'NONE', #2346, 1.500000000000001554 ) ;
#2878 = CARTESIAN_POINT ( 'NONE',  ( -43.08426400421124924, -27.08374195694514341, 1.869203119972154228E-14 ) ) ;
#2879 = VERTEX_POINT ( 'NONE', #179 ) ;
#2880 = LINE ( 'NONE', #14556, #11796 ) ;
#2881 = AXIS2_PLACEMENT_3D ( 'NONE', #15193, #7984, #1837 ) ;
#2882 = EDGE_CURVE ( 'NONE', #3698, #9058, #7770, .T. ) ;
#2883 = CARTESIAN_POINT ( 'NONE',  ( -128.0167453206627783, 9.481696373754449070, 3.150553392547042364 ) ) ;
#2884 = EDGE_CURVE ( 'NONE', #12460, #518, #18423, .T. ) ;
#2885 = CARTESIAN_POINT ( 'NONE',  ( -31.52190560670403841, -20.18723064414411894, 12.99038105676661736 ) ) ;
#2886 =( NAMED_UNIT ( * ) SI_UNIT ( $, .STERADIAN. ) SOLID_ANGLE_UNIT ( ) );
#2887 = ADVANCED_FACE ( 'NONE', ( #9260 ), #18114, .F. ) ;
#2888 = ADVANCED_FACE ( 'NONE', ( #16783 ), #13512, .F. ) ;
#2889 = AXIS2_PLACEMENT_3D ( 'NONE', #15164, #7960, #4995 ) ;
#2890 = DIRECTION ( 'NONE',  ( 0.9868632313631133801, 0.1615579233078773547, -0.000000000000000000 ) ) ;
#2891 = CARTESIAN_POINT ( 'NONE',  ( -19.38060123572413218, -23.32390534376198232, 12.99038105676661736 ) ) ;
#2892 = LINE ( 'NONE', #14566, #14076 ) ;
#2893 = CARTESIAN_POINT ( 'NONE',  ( -86.18478963674542115, 32.34879426031891114, -35.00000000000000000 ) ) ;
#2894 = ORIENTED_EDGE ( 'NONE', *, *, #1675, .F. ) ;
#2895 = CARTESIAN_POINT ( 'NONE',  ( -81.73462711737164454, 33.01666666666666572, -30.00000000000000355 ) ) ;
#2896 = CIRCLE ( 'NONE', #10158, 1.500000000000000888 ) ;
#2898 = VERTEX_POINT ( 'NONE', #659 ) ;
#2897 = CARTESIAN_POINT ( 'NONE',  ( 10.28861223506262412, -76.32329101363113466, -8.660254037844389075 ) ) ;
#2899 = ORIENTED_EDGE ( 'NONE', *, *, #11873, .T. ) ;
#2900 = ORIENTED_EDGE ( 'NONE', *, *, #15510, .F. ) ;
#2901 = CIRCLE ( 'NONE', #1127, 1.499999999999999556 ) ;
#2902 = CARTESIAN_POINT ( 'NONE',  ( -57.89905323451571206, -29.43363984018462176, 1.869203119972154228E-14 ) ) ;
#2903 = EDGE_CURVE ( 'NONE', #14167, #1906, #558, .T. ) ;
#2904 = CARTESIAN_POINT ( 'NONE',  ( -32.50955822205765600, -20.34389050302675273, 8.660254037844417496 ) ) ;
#2905 = CARTESIAN_POINT ( 'NONE',  ( -8.312069145893737243, -16.50572396040226053, 21.65063509461101177 ) ) ;
#2906 = CIRCLE ( 'NONE', #12891, 1.500000000000001332 ) ;
#2907 = DIRECTION ( 'NONE',  ( -0.1566598588826321192, 0.9876526153536342445, 7.798540720466730171E-17 ) ) ;
#2908 = DIRECTION ( 'NONE',  ( -0.9868632313631133801, -0.1615579233078775490, 0.000000000000000000 ) ) ;
#2909 = CARTESIAN_POINT ( 'NONE',  ( -46.54104815794894279, -27.63205146303435100, 8.660254037844417496 ) ) ;
#2910 = ORIENTED_EDGE ( 'NONE', *, *, #11115, .F. ) ;
#2911 = CARTESIAN_POINT ( 'NONE',  ( -25.59598991458226536, -19.24727149084832689, 8.660254037844417496 ) ) ;
#2912 = EDGE_CURVE ( 'NONE', #6362, #13731, #9458, .T. ) ;
#2913 = ADVANCED_FACE ( 'NONE', ( #7947 ), #12378, .F. ) ;
#2914 = DIRECTION ( 'NONE',  ( -0.1566598588826321747, 0.9876526153536343555, 0.000000000000000000 ) ) ;
#2915 = DIRECTION ( 'NONE',  ( -0.9876526153536341335, -0.1566598588826327021, 0.000000000000000000 ) ) ;
#2916 = VERTEX_POINT ( 'NONE', #15142 ) ;
#2917 = CIRCLE ( 'NONE', #13495, 1.499999999999999556 ) ;
#2918 = ORIENTED_EDGE ( 'NONE', *, *, #9984, .T. ) ;
#2919 = EDGE_LOOP ( 'NONE', ( #18566, #13331, #9738, #11569 ) ) ;
#2920 = ORIENTED_EDGE ( 'NONE', *, *, #10157, .T. ) ;
#2921 = CYLINDRICAL_SURFACE ( 'NONE', #1791, 1.500000000000001554 ) ;
#2922 = VECTOR ( 'NONE', #158, 1000.000000000000000 ) ;
#2923 = ORIENTED_EDGE ( 'NONE', *, *, #17865, .F. ) ;
#2924 = CIRCLE ( 'NONE', #15335, 29.12282187559191016 ) ;
#2925 = EDGE_LOOP ( 'NONE', ( #10432, #14885 ) ) ;
#2926 = DIRECTION ( 'NONE',  ( -0.1566598588826321192, 0.9876526153536342445, 7.798540720466731404E-17 ) ) ;
#2927 = CIRCLE ( 'NONE', #13510, 155.0000000000000284 ) ;
#2928 = FACE_BOUND ( 'NONE', #13748, .T. ) ;
#2929 = ORIENTED_EDGE ( 'NONE', *, *, #7920, .F. ) ;
#2930 = AXIS2_PLACEMENT_3D ( 'NONE', #5057, #2039, #12251 ) ;
#2931 = DIRECTION ( 'NONE',  ( 1.000000000000000000, 0.000000000000000000, -0.000000000000000000 ) ) ;
#2932 = ORIENTED_EDGE ( 'NONE', *, *, #15041, .T. ) ;
#2933 =( GEOMETRIC_REPRESENTATION_CONTEXT ( 3 ) GLOBAL_UNCERTAINTY_ASSIGNED_CONTEXT ( ( #14156 ) ) GLOBAL_UNIT_ASSIGNED_CONTEXT ( ( #12532, #2223, #14058 ) ) REPRESENTATION_CONTEXT ( 'NONE', 'WORKASPACE' ) );
#2934 = CARTESIAN_POINT ( 'NONE',  ( -45.01993422474066620, -85.09624311105851291, -21.65063509461098690 ) ) ;
#2935 = ORIENTED_EDGE ( 'NONE', *, *, #3430, .F. ) ;
#2936 = ADVANCED_FACE ( 'NONE', ( #6622 ), #6528, .F. ) ;
#2937 = AXIS2_PLACEMENT_3D ( 'NONE', #1093, #6865, #3611 ) ;
#2938 = LINE ( 'NONE', #8733, #13378 ) ;
#2939 = ADVANCED_FACE ( 'NONE', ( #13702 ), #5198, .F. ) ;
#2940 = DIRECTION ( 'NONE',  ( -0.9876526153536341335, -0.1566598588826327021, 0.000000000000000000 ) ) ;
#2941 = FACE_OUTER_BOUND ( 'NONE', #733, .T. ) ;
#2942 = LINE ( 'NONE', #11732, #10555 ) ;
#2943 = AXIS2_PLACEMENT_3D ( 'NONE', #13566, #10718, #2114 ) ;
#2944 = FACE_OUTER_BOUND ( 'NONE', #18556, .T. ) ;
#2945 = ADVANCED_FACE ( 'NONE', ( #9080 ), #3374, .F. ) ;
#2946 = VERTEX_POINT ( 'NONE', #9181 ) ;
#2947 = ORIENTED_EDGE ( 'NONE', *, *, #10175, .T. ) ;
#2948 = ORIENTED_EDGE ( 'NONE', *, *, #10985, .F. ) ;
#2949 = DIRECTION ( 'NONE',  ( 0.000000000000000000, 0.000000000000000000, 1.000000000000000000 ) ) ;
#2950 = EDGE_LOOP ( 'NONE', ( #7070, #12584, #14818, #11398 ) ) ;
#2951 = CARTESIAN_POINT ( 'NONE',  ( -309.1404785418517918, -2.850701963179328668, 12.83663829214476237 ) ) ;
#2952 = AXIS2_PLACEMENT_3D ( 'NONE', #18531, #2551, #3760 ) ;
#2953 = LINE ( 'NONE', #11296, #903 ) ;
#2954 = EDGE_LOOP ( 'NONE', ( #14575, #6574, #14958, #16245 ) ) ;
#2955 = DIRECTION ( 'NONE',  ( -0.1566598588826321192, 0.9876526153536342445, 7.798540720466731404E-17 ) ) ;
#2956 = SHAPE_DEFINITION_REPRESENTATION ( #3460, #10585 ) ;
#2957 = CARTESIAN_POINT ( 'NONE',  ( -8.476787456656362352, -79.29982833240114815, -21.65063509461098690 ) ) ;
#2958 = VECTOR ( 'NONE', #13636, 1000.000000000000000 ) ;
#2959 = AXIS2_PLACEMENT_3D ( 'NONE', #17065, #4236, #11608 ) ;
#2960 = CARTESIAN_POINT ( 'NONE',  ( -51.27495791377661760, -23.32042782179675200, 12.99038105676661736 ) ) ;
#2961 = DIRECTION ( 'NONE',  ( -0.1566598588826321192, 0.9876526153536342445, 7.798540720466730171E-17 ) ) ;
#2962 = AXIS2_PLACEMENT_3D ( 'NONE', #11344, #1426, #8893 ) ;
#2963 = CARTESIAN_POINT ( 'NONE',  ( -88.52719037593115559, 10.14639200037310296, -20.00000000000001066 ) ) ;
#2964 = ORIENTED_EDGE ( 'NONE', *, *, #17775, .T. ) ;
#2965 = VERTEX_POINT ( 'NONE', #747 ) ;
#2966 = CARTESIAN_POINT ( 'NONE',  ( 0.000000000000000000, 0.000000000000000000, 25.00000000000000000 ) ) ;
#2967 = EDGE_CURVE ( 'NONE', #13690, #14963, #3552, .T. ) ;
#2968 = DIRECTION ( 'NONE',  ( -0.9876526153536341335, -0.1566598588826327021, 0.000000000000000000 ) ) ;
#2969 = DIRECTION ( 'NONE',  ( -0.1566598588826321192, 0.9876526153536342445, 7.798540720466731404E-17 ) ) ;
#2970 = AXIS2_PLACEMENT_3D ( 'NONE', #2966, #4104, #141 ) ;
#2971 = ORIENTED_EDGE ( 'NONE', *, *, #191, .T. ) ;
#2972 = DIRECTION ( 'NONE',  ( -0.1566598588826321192, 0.9876526153536342445, 7.798540720466730171E-17 ) ) ;
#2973 = EDGE_CURVE ( 'NONE', #16508, #13410, #8109, .T. ) ;
#2974 = ORIENTED_EDGE ( 'NONE', *, *, #11771, .T. ) ;
#2975 = CIRCLE ( 'NONE', #10242, 1.500000000000000444 ) ;
#2976 = CIRCLE ( 'NONE', #1200, 1.500000000000000888 ) ;
#2977 = DIRECTION ( 'NONE',  ( -0.1566598588826321747, 0.9876526153536343555, 0.000000000000000000 ) ) ;
#2978 = CARTESIAN_POINT ( 'NONE',  ( -51.97313754239392125, -28.49368068688882261, 12.99038105676661736 ) ) ;
#2979 = CARTESIAN_POINT ( 'NONE',  ( -84.20693962813486166, 32.64562644091790844, -35.00000000000000000 ) ) ;
#2980 = ORIENTED_EDGE ( 'NONE', *, *, #492, .T. ) ;
#2981 = VECTOR ( 'NONE', #14334, 1000.000000000000000 ) ;
#2982 = FACE_OUTER_BOUND ( 'NONE', #15483, .T. ) ;
#2983 = ADVANCED_FACE ( 'NONE', ( #13615 ), #10756, .F. ) ;
#2985 = LINE ( 'NONE', #17248, #2922 ) ;
#2984 = CIRCLE ( 'NONE', #13574, 1.500000000000001332 ) ;
#2986 = PLANE ( 'NONE',  #12549 ) ;
#2987 = CIRCLE ( 'NONE', #8458, 1.500000000000000888 ) ;
#2988 = EDGE_LOOP ( 'NONE', ( #6583, #13387, #15258, #4299 ) ) ;
#2989 = LINE ( 'NONE', #7377, #6400 ) ;
#2990 = VERTEX_POINT ( 'NONE', #12184 ) ;
#2991 = CIRCLE ( 'NONE', #16020, 1.499999999999999556 ) ;
#2993 = EDGE_LOOP ( 'NONE', ( #10365, #3487, #195, #4253 ) ) ;
#2992 = CYLINDRICAL_SURFACE ( 'NONE', #11129, 1.500000000000001554 ) ;
#2994 = EDGE_CURVE ( 'NONE', #1938, #9527, #4772, .T. ) ;
#2995 = EDGE_CURVE ( 'NONE', #999, #12526, #12653, .T. ) ;
#2996 = DIRECTION ( 'NONE',  ( -0.1566598588826321747, 0.9876526153536343555, 0.000000000000000000 ) ) ;
#2997 = EDGE_LOOP ( 'NONE', ( #16490, #7785 ) ) ;
#2998 = EDGE_CURVE ( 'NONE', #7107, #13776, #10226, .T. ) ;
#2999 = ORIENTED_EDGE ( 'NONE', *, *, #14727, .T. ) ;
#3000 = AXIS2_PLACEMENT_3D ( 'NONE', #6875, #5042, #5156 ) ;
#3001 = AXIS2_PLACEMENT_3D ( 'NONE', #3771, #13725, #6472 ) ;
#3002 = DIRECTION ( 'NONE',  ( -0.1566598588826321192, 0.9876526153536342445, 7.798540720466731404E-17 ) ) ;
#3003 = CIRCLE ( 'NONE', #7565, 1.500000000000000888 ) ;
#3004 = CARTESIAN_POINT ( 'NONE',  ( -66.25446545484369665, -88.46443007703511796, -12.99038105676658539 ) ) ;
#3005 = DIRECTION ( 'NONE',  ( 8.693966348389027220E-17, -1.991237296706374949E-16, 1.000000000000000000 ) ) ;
#3006 = AXIS2_PLACEMENT_3D ( 'NONE', #17654, #7826, #14674 ) ;
#3007 = CIRCLE ( 'NONE', #7557, 1.500000000000000444 ) ;
#3008 = EDGE_LOOP ( 'NONE', ( #16125, #14065, #17785, #18030 ) ) ;
#3009 = CARTESIAN_POINT ( 'NONE',  ( -44.85521591397802155, -22.30213873905965016, 12.99038105676661736 ) ) ;
#3010 = LINE ( 'NONE', #12955, #8538 ) ;
#3011 = LINE ( 'NONE', #7215, #15376 ) ;
#3012 = DIRECTION ( 'NONE',  ( 1.000000000000000000, 0.000000000000000000, 0.000000000000000000 ) ) ;
#3013 = ORIENTED_EDGE ( 'NONE', *, *, #1702, .T. ) ;
#3014 = CARTESIAN_POINT ( 'NONE',  ( 0.000000000000000000, 0.000000000000000000, 20.00000000000000000 ) ) ;
#3015 = FACE_BOUND ( 'NONE', #3640, .T. ) ;
#3016 = CIRCLE ( 'NONE', #16041, 1.500000000000001332 ) ;
#3017 = LINE ( 'NONE', #16196, #12595 ) ;
#3018 = CIRCLE ( 'NONE', #12071, 1.500000000000000000 ) ;
#3019 = ADVANCED_FACE ( 'NONE', ( #4031 ), #15601, .T. ) ;
#3020 = ORIENTED_EDGE ( 'NONE', *, *, #9089, .T. ) ;
#3021 = CIRCLE ( 'NONE', #13014, 1.500000000000000888 ) ;
#3023 = ORIENTED_EDGE ( 'NONE', *, *, #787, .T. ) ;
#3022 = EDGE_CURVE ( 'NONE', #11092, #17712, #18438, .T. ) ;
#3024 = CARTESIAN_POINT ( 'NONE',  ( -32.67427653282027933, -83.13799487502562613, 17.32050807568881368 ) ) ;
#3025 = VECTOR ( 'NONE', #709, 1000.000000000000000 ) ;
#3026 = ORIENTED_EDGE ( 'NONE', *, *, #13251, .F. ) ;
#3027 = ORIENTED_EDGE ( 'NONE', *, *, #1494, .F. ) ;
#3028 = DIRECTION ( 'NONE',  ( -0.1566598588826321192, 0.9876526153536342445, 7.798540720466731404E-17 ) ) ;
#3029 = DIRECTION ( 'NONE',  ( -0.1566598588826321192, 0.9876526153536342445, 7.798540720466731404E-17 ) ) ;
#3030 = EDGE_LOOP ( 'NONE', ( #8367, #11077 ) ) ;
#3031 = CIRCLE ( 'NONE', #13614, 1.500000000000001332 ) ;
#3032 = DIRECTION ( 'NONE',  ( -0.9876526153536341335, -0.1566598588826327021, 0.000000000000000000 ) ) ;
#3033 = CIRCLE ( 'NONE', #1540, 1.500000000000000000 ) ;
#3034 = EDGE_LOOP ( 'NONE', ( #16222, #15224, #6139, #16013 ) ) ;
#3035 = AXIS2_PLACEMENT_3D ( 'NONE', #10057, #8460, #11560 ) ;
#3036 = CARTESIAN_POINT ( 'NONE',  ( -129.1404785418517918, -14.35070196317933267, -5.500000000000000000 ) ) ;
#3037 = CIRCLE ( 'NONE', #9719, 171.3327290851023292 ) ;
#3038 = DIRECTION ( 'NONE',  ( 0.000000000000000000, 0.000000000000000000, 1.000000000000000000 ) ) ;
#3039 = VECTOR ( 'NONE', #11130, 1000.000000000000000 ) ;
#3040 = EDGE_LOOP ( 'NONE', ( #6079, #12116 ) ) ;
#3041 = FACE_BOUND ( 'NONE', #12525, .T. ) ;
#3042 = FACE_OUTER_BOUND ( 'NONE', #3280, .T. ) ;
#3043 = ORIENTED_EDGE ( 'NONE', *, *, #14558, .F. ) ;
#3044 = DIRECTION ( 'NONE',  ( 1.000000000000000000, 0.000000000000000000, 0.000000000000000000 ) ) ;
#3045 = DIRECTION ( 'NONE',  ( -0.1566598588826321192, 0.9876526153536342445, 7.798540720466730171E-17 ) ) ;
#3046 = FACE_OUTER_BOUND ( 'NONE', #2606, .T. ) ;
#3047 = AXIS2_PLACEMENT_3D ( 'NONE', #5656, #18602, #5474 ) ;
#3048 = DIRECTION ( 'NONE',  ( -0.9876526153536341335, -0.1566598588826327021, 0.000000000000000000 ) ) ;
#3049 = AXIS2_PLACEMENT_3D ( 'NONE', #16181, #3261, #7554 ) ;
#3050 = ORIENTED_EDGE ( 'NONE', *, *, #11365, .T. ) ;
#3051 = EDGE_LOOP ( 'NONE', ( #594, #13177, #15838, #8981 ) ) ;
#3052 = ORIENTED_EDGE ( 'NONE', *, *, #7099, .F. ) ;
#3053 = ORIENTED_EDGE ( 'NONE', *, *, #9542, .T. ) ;
#3054 = CARTESIAN_POINT ( 'NONE',  ( -129.1404785418517918, -2.850701963179328668, 9.951701414186818625E-16 ) ) ;
#3055 = EDGE_CURVE ( 'NONE', #7702, #344, #2623, .T. ) ;
#3056 = VECTOR ( 'NONE', #4496, 1000.000000000000000 ) ;
#3057 = DIRECTION ( 'NONE',  ( -0.1566598588826321192, 0.9876526153536342445, 7.798540720466731404E-17 ) ) ;
#3058 = EDGE_CURVE ( 'NONE', #62, #14796, #11979, .T. ) ;
#3059 = ORIENTED_EDGE ( 'NONE', *, *, #15182, .T. ) ;
#3060 = VERTEX_POINT ( 'NONE', #9914 ) ;
#3061 = ADVANCED_FACE ( 'NONE', ( #11418 ), #3510, .T. ) ;
#3062 = EDGE_LOOP ( 'NONE', ( #8219, #13627 ) ) ;
#3063 = AXIS2_PLACEMENT_3D ( 'NONE', #4292, #10068, #12714 ) ;
#3064 = CYLINDRICAL_SURFACE ( 'NONE', #10599, 1.500000000000000888 ) ;
#3065 = DIRECTION ( 'NONE',  ( -0.1566598588826321192, 0.9876526153536342445, 7.798540720466730171E-17 ) ) ;
#3066 = CARTESIAN_POINT ( 'NONE',  ( -174.8824303167912717, 55.30300876447670788, -5.132104245558540612 ) ) ;
#3067 = CARTESIAN_POINT ( 'NONE',  ( -71.14323843904776368, 45.48645312032893173, -4.192014029982320977 ) ) ;
#3068 = CARTESIAN_POINT ( 'NONE',  ( -54.44226908077801141, -28.88533033409540351, 1.869203119972154228E-14 ) ) ;
#3069 = ORIENTED_EDGE ( 'NONE', *, *, #16811, .T. ) ;
#3070 = VERTEX_POINT ( 'NONE', #8130 ) ;
#3071 = CYLINDRICAL_SURFACE ( 'NONE', #15386, 1.500000000000001554 ) ;
#3072 = CARTESIAN_POINT ( 'NONE',  ( -13.45468554360235203, -22.38394619046619383, -17.32050807568878170 ) ) ;
#3073 = CIRCLE ( 'NONE', #17644, 1.500000000000000000 ) ;
#3074 = EDGE_LOOP ( 'NONE', ( #6524, #10962, #2478, #2775 ) ) ;
#3075 = EDGE_LOOP ( 'NONE', ( #14299, #12328 ) ) ;
#3076 = CARTESIAN_POINT ( 'NONE',  ( -58.88670584986932965, -29.59029969906724844, -4.330127018922181215 ) ) ;
#3077 = CIRCLE ( 'NONE', #5199, 2.000000000000000000 ) ;
#3078 = CARTESIAN_POINT ( 'NONE',  ( -39.13365354279672204, -26.45710252141460828, -4.330127018922181215 ) ) ;
#3079 = EDGE_CURVE ( 'NONE', #1095, #5465, #1442, .T. ) ;
#3080 = DIRECTION ( 'NONE',  ( 0.000000000000000000, 0.000000000000000000, 1.000000000000000000 ) ) ;
#3081 = FILL_AREA_STYLE_COLOUR ( '', #13822 ) ;
#3082 = DIRECTION ( 'NONE',  ( -0.1566598588826321192, 0.9876526153536342445, 7.798540720466730171E-17 ) ) ;
#3083 = DIRECTION ( 'NONE',  ( -0.000000000000000000, -0.000000000000000000, -1.000000000000000000 ) ) ;
#3084 = ADVANCED_FACE ( 'NONE', ( #5289 ), #3941, .F. ) ;
#3085 = CYLINDRICAL_SURFACE ( 'NONE', #6836, 1.500000000000001554 ) ;
#3086 = ORIENTED_EDGE ( 'NONE', *, *, #11575, .F. ) ;
#3087 = ORIENTED_EDGE ( 'NONE', *, *, #4173, .F. ) ;
#3088 = VECTOR ( 'NONE', #14399, 1000.000000000000000 ) ;
#3089 = CARTESIAN_POINT ( 'NONE',  ( -23.12685837619818940, -18.85562184364174598, 21.65063509461101177 ) ) ;
#3090 = ORIENTED_EDGE ( 'NONE', *, *, #467, .F. ) ;
#3091 = ORIENTED_EDGE ( 'NONE', *, *, #15821, .T. ) ;
#3092 = CARTESIAN_POINT ( 'NONE',  ( -60.36818477289978091, -29.82528948739120267, -21.65063509461098334 ) ) ;
#3093 = VERTEX_POINT ( 'NONE', #11243 ) ;
#3094 = EDGE_LOOP ( 'NONE', ( #10235, #15609 ) ) ;
#3095 = ORIENTED_EDGE ( 'NONE', *, *, #387, .T. ) ;
#3096 = CARTESIAN_POINT ( 'NONE',  ( 9.300959619709004755, -76.47995087251376845, -4.330127018922189208 ) ) ;
#3097 = DIRECTION ( 'NONE',  ( -0.1566598588826321747, 0.9876526153536343555, 0.000000000000000000 ) ) ;
#3098 = EDGE_CURVE ( 'NONE', #3317, #14743, #15520, .T. ) ;
#3099 = CARTESIAN_POINT ( 'NONE',  ( -20.32861884089991023, -81.17974663899273935, 12.99038105676661203 ) ) ;
#3100 = CARTESIAN_POINT ( 'NONE',  ( -5.059638313096497697, -21.05233738996382797, -8.660254037844383745 ) ) ;
#3101 = CARTESIAN_POINT ( 'NONE',  ( -75.18297400320422241, -32.17518737063066681, 12.99038105676661736 ) ) ;
#3102 = FACE_OUTER_BOUND ( 'NONE', #193, .T. ) ;
#3103 = DIRECTION ( 'NONE',  ( -0.1566598588826321192, 0.9876526153536342445, 7.798540720466730171E-17 ) ) ;
#3104 = DIRECTION ( 'NONE',  ( -0.1566598588826321747, 0.9876526153536343555, 0.000000000000000000 ) ) ;
#3105 = ADVANCED_FACE ( 'NONE', ( #16971 ), #17062, .F. ) ;
#3106 = DIRECTION ( 'NONE',  ( -0.9876526153536341335, -0.1566598588826327021, 0.000000000000000000 ) ) ;
#3107 = DIRECTION ( 'NONE',  ( 0.000000000000000000, 0.000000000000000000, -1.000000000000000000 ) ) ;
#3109 = ORIENTED_EDGE ( 'NONE', *, *, #15067, .F. ) ;
#3108 = LINE ( 'NONE', #8899, #16953 ) ;
#3110 = ORIENTED_EDGE ( 'NONE', *, *, #13827, .F. ) ;
#3111 = EDGE_LOOP ( 'NONE', ( #12315, #6151, #1508, #14266 ) ) ;
#3112 = DIRECTION ( 'NONE',  ( -0.1566598588826321192, 0.9876526153536342445, 7.798540720466730171E-17 ) ) ;
#3113 = CIRCLE ( 'NONE', #3399, 1.500000000000000000 ) ;
#3114 = ORIENTED_EDGE ( 'NONE', *, *, #8242, .F. ) ;
#3115 = ORIENTED_EDGE ( 'NONE', *, *, #11766, .T. ) ;
#3116 = CARTESIAN_POINT ( 'NONE',  ( -4.361458684479201153, -15.87908452487173427, 17.32050807568881368 ) ) ;
#3117 = EDGE_CURVE ( 'NONE', #4380, #6069, #9755, .T. ) ;
#3118 = FACE_OUTER_BOUND ( 'NONE', #4884, .T. ) ;
#3119 = EDGE_CURVE ( 'NONE', #5990, #11990, #7201, .T. ) ;
#3120 = CARTESIAN_POINT ( 'NONE',  ( -33.99103714508810725, -20.57888029135069630, 8.660254037844417496 ) ) ;
#3121 = EDGE_LOOP ( 'NONE', ( #13324, #1618, #17761, #5458 ) ) ;
#3122 = EDGE_CURVE ( 'NONE', #4463, #16997, #17479, .T. ) ;
#3123 = EDGE_CURVE ( 'NONE', #753, #7914, #8693, .T. ) ;
#3124 = CIRCLE ( 'NONE', #9481, 1.500000000000000000 ) ;
#3125 = EDGE_CURVE ( 'NONE', #10450, #11814, #7477, .T. ) ;
#3126 = EDGE_LOOP ( 'NONE', ( #3180, #13855 ) ) ;
#3127 = VERTEX_POINT ( 'NONE', #2724 ) ;
#3128 = DIRECTION ( 'NONE',  ( -0.1566598588826321747, 0.9876526153536343555, 0.000000000000000000 ) ) ;
#3129 = DIRECTION ( 'NONE',  ( -1.000000000000000000, 0.000000000000000000, 0.000000000000000000 ) ) ;
#3130 = DIRECTION ( 'NONE',  ( -0.1566598588826321192, 0.9876526153536342445, 7.798540720466730171E-17 ) ) ;
#3131 = ORIENTED_EDGE ( 'NONE', *, *, #14004, .F. ) ;
#3132 = ORIENTED_EDGE ( 'NONE', *, *, #8587, .F. ) ;
#3133 = ORIENTED_EDGE ( 'NONE', *, *, #11487, .T. ) ;
#3134 = ORIENTED_EDGE ( 'NONE', *, *, #3540, .T. ) ;
#3135 = CARTESIAN_POINT ( 'NONE',  ( -46.54104815794894279, -27.63205146303435100, 17.32050807568881723 ) ) ;
#3136 = FACE_BOUND ( 'NONE', #15085, .T. ) ;
#3137 = DIRECTION ( 'NONE',  ( 0.000000000000000000, 0.000000000000000000, 1.000000000000000000 ) ) ;
#3138 = VERTEX_POINT ( 'NONE', #17523 ) ;
#3139 = CARTESIAN_POINT ( 'NONE',  ( -21.84973277410820458, -23.71555499096855613, -8.660254037844380193 ) ) ;
#3140 = ORIENTED_EDGE ( 'NONE', *, *, #6747, .F. ) ;
#3141 = EDGE_LOOP ( 'NONE', ( #2632, #13388, #18583, #396 ) ) ;
#3142 = FACE_BOUND ( 'NONE', #4869, .T. ) ;
#3143 = ORIENTED_EDGE ( 'NONE', *, *, #15952, .T. ) ;
#3144 = CARTESIAN_POINT ( 'NONE',  ( -53.74408945216070776, -23.71207746900332580, 1.908195823574487804E-14 ) ) ;
#3145 = CARTESIAN_POINT ( 'NONE',  ( -17.40529600501688279, -23.01058562599671831, 21.65063509461101177 ) ) ;
#3146 = EDGE_CURVE ( 'NONE', #855, #2319, #350, .T. ) ;
#3147 = DIRECTION ( 'NONE',  ( 1.000000000000000000, 0.000000000000000000, 0.000000000000000000 ) ) ;
#3148 = DIRECTION ( 'NONE',  ( 0.9201637183752249260, 0.3915338189555018777, -2.458192809297183803E-16 ) ) ;
#3149 = ORIENTED_EDGE ( 'NONE', *, *, #17512, .F. ) ;
#3150 = EDGE_CURVE ( 'NONE', #8286, #4960, #6034, .T. ) ;
#3151 = ORIENTED_EDGE ( 'NONE', *, *, #3615, .T. ) ;
#3152 = DIRECTION ( 'NONE',  ( -0.9876526153536336894, -0.1566598588826349503, 0.000000000000000000 ) ) ;
#3153 = AXIS2_PLACEMENT_3D ( 'NONE', #2089, #10332, #9110 ) ;
#3154 = LINE ( 'NONE', #1479, #2643 ) ;
#3155 = FACE_OUTER_BOUND ( 'NONE', #8925, .T. ) ;
#3156 = EDGE_LOOP ( 'NONE', ( #12323, #13204, #7873, #9776 ) ) ;
#3157 = DIRECTION ( 'NONE',  ( -0.1566598588826321192, 0.9876526153536342445, 7.798540720466731404E-17 ) ) ;
#3158 = CIRCLE ( 'NONE', #1092, 2.200000000000000178 ) ;
#3159 = DIRECTION ( 'NONE',  ( -0.1566598588826321192, 0.9876526153536342445, 7.798540720466730171E-17 ) ) ;
#3160 = DIRECTION ( 'NONE',  ( -0.1615579233078772992, -0.9868632313631134911, 0.000000000000000000 ) ) ;
#3161 = VERTEX_POINT ( 'NONE', #10188 ) ;
#3162 = DIRECTION ( 'NONE',  ( -1.000000000000000000, 0.000000000000000000, 0.000000000000000000 ) ) ;
#3163 = PRESENTATION_STYLE_ASSIGNMENT (( #9236 ) ) ;
#3164 = ADVANCED_FACE ( 'NONE', ( #6138 ), #75, .F. ) ;
#3165 = CARTESIAN_POINT ( 'NONE',  ( -43.86756329862441817, -22.14547888017700572, -8.660254037844380193 ) ) ;
#3166 = CARTESIAN_POINT ( 'NONE',  ( 0.4120860815263194254, -77.88988960245745830, -8.660254037844385522 ) ) ;
#3167 = ORIENTED_EDGE ( 'NONE', *, *, #11156, .T. ) ;
#3168 = CARTESIAN_POINT ( 'NONE',  ( -66.08974714408107332, -25.67032570503623035, 21.65063509461102242 ) ) ;
#3169 = VERTEX_POINT ( 'NONE', #8611 ) ;
#3170 = EDGE_CURVE ( 'NONE', #15663, #4041, #3823, .T. ) ;
#3171 = AXIS2_PLACEMENT_3D ( 'NONE', #14041, #13843, #12320 ) ;
#3172 = ORIENTED_EDGE ( 'NONE', *, *, #13765, .T. ) ;
#3173 = CYLINDRICAL_SURFACE ( 'NONE', #8496, 1.500000000000001554 ) ;
#3174 = CARTESIAN_POINT ( 'NONE',  ( -27.28182215855319015, -24.57718421482303484, 4.330127018922217630 ) ) ;
#3175 = VERTEX_POINT ( 'NONE', #4231 ) ;
#3176 = CARTESIAN_POINT ( 'NONE',  ( -69.99999999999998579, -45.00000000000000711, 20.00000000000001776 ) ) ;
#3177 = AXIS2_PLACEMENT_3D ( 'NONE', #5182, #10943, #16770 ) ;
#3178 = LINE ( 'NONE', #3099, #11292 ) ;
#3179 = CARTESIAN_POINT ( 'NONE',  ( -4.526176995241833367, -78.67318889687062722, 8.660254037844408614 ) ) ;
#3180 = ORIENTED_EDGE ( 'NONE', *, *, #8240, .T. ) ;
#3181 = DIRECTION ( 'NONE',  ( -0.1566598588826321192, 0.9876526153536342445, 7.798540720466730171E-17 ) ) ;
#3182 = DIRECTION ( 'NONE',  ( -0.9998476951563911586, 0.000000000000000000, 0.01745240643728354635 ) ) ;
#3183 = AXIS2_PLACEMENT_3D ( 'NONE', #16892, #16989, #8345 ) ;
#3184 = ORIENTED_EDGE ( 'NONE', *, *, #8240, .F. ) ;
#3185 = DIRECTION ( 'NONE',  ( -0.1566598588826321747, 0.9876526153536343555, 0.000000000000000000 ) ) ;
#3186 = DIRECTION ( 'NONE',  ( -0.9876526153536341335, -0.1566598588826327021, 0.000000000000000000 ) ) ;
#3187 = EDGE_LOOP ( 'NONE', ( #7835, #12831, #11103, #4991, #2315, #2899 ) ) ;
#3188 = EDGE_LOOP ( 'NONE', ( #15172, #10918, #18610 ) ) ;
#3189 = EDGE_LOOP ( 'NONE', ( #9506, #18693, #12711, #10744 ) ) ;
#3190 = CARTESIAN_POINT ( 'NONE',  ( -68.76323200340563346, -31.15689828789355786, 12.99038105676661736 ) ) ;
#3191 = ORIENTED_EDGE ( 'NONE', *, *, #1172, .F. ) ;
#3192 = CIRCLE ( 'NONE', #11953, 1.500000000000001332 ) ;
#3193 = EDGE_CURVE ( 'NONE', #14599, #2583, #14384, .T. ) ;
#3194 = ORIENTED_EDGE ( 'NONE', *, *, #12968, .T. ) ;
#3195 = VERTEX_POINT ( 'NONE', #7193 ) ;
#3196 = ORIENTED_EDGE ( 'NONE', *, *, #9202, .T. ) ;
#3197 = DIRECTION ( 'NONE',  ( 0.1856185419698760941, -0.9826218788918640312, 0.000000000000000000 ) ) ;
#3198 = CIRCLE ( 'NONE', #5352, 1.500000000000000444 ) ;
#3199 = EDGE_LOOP ( 'NONE', ( #3658, #8523, #17690, #129 ) ) ;
#3200 = DIRECTION ( 'NONE',  ( 8.693966348389027220E-17, -1.991237296706374949E-16, 1.000000000000000000 ) ) ;
#3201 = EDGE_CURVE ( 'NONE', #9794, #12027, #14443, .T. ) ;
#3202 = DIRECTION ( 'NONE',  ( -0.1566598588826321192, 0.9876526153536342445, 7.798540720466731404E-17 ) ) ;
#3203 = DIRECTION ( 'NONE',  ( -0.1566598588826321192, 0.9876526153536342445, 7.798540720466731404E-17 ) ) ;
#3204 = ORIENTED_EDGE ( 'NONE', *, *, #4750, .F. ) ;
#3205 = CIRCLE ( 'NONE', #13799, 1.499999999999999556 ) ;
#3206 = DIRECTION ( 'NONE',  ( -0.1566598588826321192, 0.9876526153536342445, 7.798540720466730171E-17 ) ) ;
#3207 = CYLINDRICAL_SURFACE ( 'NONE', #1815, 1.500000000000001554 ) ;
#3208 = DIRECTION ( 'NONE',  ( -0.1566598588826321192, 0.9876526153536342445, 7.798540720466731404E-17 ) ) ;
#3209 = ORIENTED_EDGE ( 'NONE', *, *, #18358, .F. ) ;
#3210 = PRESENTATION_STYLE_ASSIGNMENT (( #14519 ) ) ;
#3211 = ORIENTED_EDGE ( 'NONE', *, *, #1319, .T. ) ;
#3212 = CARTESIAN_POINT ( 'NONE',  ( 0.000000000000000000, 0.000000000000000000, -20.00000000000000355 ) ) ;
#3213 = MECHANICAL_DESIGN_GEOMETRIC_PRESENTATION_REPRESENTATION (  '', ( #11387 ), #8064 ) ;
#3214 = DIRECTION ( 'NONE',  ( -0.1566598588826321192, 0.9876526153536342445, 7.798540720466730171E-17 ) ) ;
#3215 = ORIENTED_EDGE ( 'NONE', *, *, #7887, .F. ) ;
#3216 = EDGE_LOOP ( 'NONE', ( #16551, #503, #8590, #10451 ) ) ;
#3217 = EDGE_LOOP ( 'NONE', ( #14505, #4465, #354, #5009 ) ) ;
#3218 = DIRECTION ( 'NONE',  ( -0.1566598588826321192, 0.9876526153536342445, 7.798540720466731404E-17 ) ) ;
#3219 = ADVANCED_FACE ( 'NONE', ( #10289 ), #1672, .F. ) ;
#3220 = EDGE_CURVE ( 'NONE', #12815, #17451, #5025, .T. ) ;
#3221 = FACE_BOUND ( 'NONE', #15340, .T. ) ;
#3222 = EDGE_CURVE ( 'NONE', #11890, #16742, #829, .T. ) ;
#3223 = DIRECTION ( 'NONE',  ( -0.9876526153536341335, -0.1566598588826327021, 0.000000000000000000 ) ) ;
#3224 = ORIENTED_EDGE ( 'NONE', *, *, #16168, .F. ) ;
#3225 =( NAMED_UNIT ( * ) SI_UNIT ( $, .STERADIAN. ) SOLID_ANGLE_UNIT ( ) );
#3226 =( GEOMETRIC_REPRESENTATION_CONTEXT ( 3 ) GLOBAL_UNCERTAINTY_ASSIGNED_CONTEXT ( ( #4915 ) ) GLOBAL_UNIT_ASSIGNED_CONTEXT ( ( #1474, #15867, #11213 ) ) REPRESENTATION_CONTEXT ( 'NONE', 'WORKASPACE' ) );
#3227 = VERTEX_POINT ( 'NONE', #4413 ) ;
#3228 = AXIS2_PLACEMENT_3D ( 'NONE', #4904, #9463, #7856 ) ;
#3229 = VERTEX_POINT ( 'NONE', #4330 ) ;
#3230 = VERTEX_POINT ( 'NONE', #15890 ) ;
#3231 = AXIS2_PLACEMENT_3D ( 'NONE', #15088, #4857, #16443 ) ;
#3232 = CARTESIAN_POINT ( 'NONE',  ( -41.56315007100295844, -84.54793360496931598, -4.330127018922185655 ) ) ;
#3233 = DIRECTION ( 'NONE',  ( -0.1566598588826321747, 0.9876526153536343555, 0.000000000000000000 ) ) ;
#3234 = CARTESIAN_POINT ( 'NONE',  ( -41.56315007100295844, -84.54793360496931598, 4.330127018922213189 ) ) ;
#3235 = DIRECTION ( 'NONE',  ( -0.1566598588826321192, 0.9876526153536342445, 7.798540720466730171E-17 ) ) ;
#3236 = CARTESIAN_POINT ( 'NONE',  ( -12.46703292824873088, -22.22728633158356359, -4.330127018922181215 ) ) ;
#3237 = ORIENTED_EDGE ( 'NONE', *, *, #15177, .T. ) ;
#3238 = EDGE_LOOP ( 'NONE', ( #8742, #3638, #9483, #17486 ) ) ;
#3239 = CARTESIAN_POINT ( 'NONE',  ( -47.81817376003895248, -22.77211831570752665, -21.65063509461098334 ) ) ;
#3240 = DIRECTION ( 'NONE',  ( -0.1566598588826321192, 0.9876526153536342445, 7.798540720466730171E-17 ) ) ;
#3241 = AXIS2_PLACEMENT_3D ( 'NONE', #13667, #16244, #3242 ) ;
#3242 = DIRECTION ( 'NONE',  ( 0.000000000000000000, 0.000000000000000000, 1.000000000000000000 ) ) ;
#3243 = ADVANCED_FACE ( 'NONE', ( #13217 ), #246, .T. ) ;
#3244 = APPLICATION_CONTEXT ( 'automotive_design' ) ;
#3245 = ORIENTED_EDGE ( 'NONE', *, *, #15359, .F. ) ;
#3246 = DIRECTION ( 'NONE',  ( -0.1566598588826321192, 0.9876526153536342445, 7.798540720466731404E-17 ) ) ;
#3247 = AXIS2_PLACEMENT_3D ( 'NONE', #10957, #4801, #10592 ) ;
#3248 = ADVANCED_FACE ( 'NONE', ( #17629 ), #1760, .F. ) ;
#3249 = DIRECTION ( 'NONE',  ( 1.000000000000000000, 0.000000000000000000, -2.671473304378624222E-16 ) ) ;
#3250 = CIRCLE ( 'NONE', #15106, 1.499999999999999556 ) ;
#3251 = DIRECTION ( 'NONE',  ( 0.000000000000000000, 0.000000000000000000, 1.000000000000000000 ) ) ;
#3252 = DIRECTION ( 'NONE',  ( -0.1566598588826321747, 0.9876526153536343555, 0.000000000000000000 ) ) ;
#3253 =( NAMED_UNIT ( * ) PLANE_ANGLE_UNIT ( ) SI_UNIT ( $, .RADIAN. ) );
#3254 = AXIS2_PLACEMENT_3D ( 'NONE', #6643, #9769, #9566 ) ;
#3255 = ORIENTED_EDGE ( 'NONE', *, *, #13564, .F. ) ;
#3256 = CARTESIAN_POINT ( 'NONE',  ( -58.68235252892885256, -24.49537676341648762, 8.660254037844417496 ) ) ;
#3257 = DIRECTION ( 'NONE',  ( -0.9876526153536336894, -0.1566598588826349503, 0.000000000000000000 ) ) ;
#3258 = CARTESIAN_POINT ( 'NONE',  ( -42.09661138885763165, -26.92708209806250608, 12.99038105676661736 ) ) ;
#3259 = VERTEX_POINT ( 'NONE', #13403 ) ;
#3260 = EDGE_LOOP ( 'NONE', ( #16369, #2026 ) ) ;
#3261 = DIRECTION ( 'NONE',  ( -0.1566598588826321747, 0.9876526153536343555, 0.000000000000000000 ) ) ;
#3262 = CONICAL_SURFACE ( 'NONE', #5717, 15.74754878398195856, 0.01745329251994333364 ) ;
#3263 = VERTEX_POINT ( 'NONE', #11957 ) ;
#3264 = CIRCLE ( 'NONE', #10820, 1.500000000000000888 ) ;
#3265 = ORIENTED_EDGE ( 'NONE', *, *, #18344, .T. ) ;
#3266 = DIRECTION ( 'NONE',  ( -0.1566598588826321192, 0.9876526153536342445, 7.798540720466731404E-17 ) ) ;
#3267 = EDGE_CURVE ( 'NONE', #11861, #13426, #2628, .T. ) ;
#3268 = CLOSED_SHELL ( 'NONE', ( #9951, #4039, #1012, #1071, #1793, #1628, #5538, #10881, #3871, #14129, #18595, #12794, #85, #10346, #8273, #12172, #5357, #1718, #11643, #9411, #18632, #634, #13985, #3105, #4856, #13649, #18487, #1627, #18382, #14420, #13554, #13698, #12325, #5455, #11741, #8566, #11712, #11441, #2208, #7666, #18748, #3243, #13478, #7173, #7750, #17276, #15621 ) ) ;
#3269 = EDGE_CURVE ( 'NONE', #5005, #13430, #10487, .T. ) ;
#3270 = FACE_OUTER_BOUND ( 'NONE', #15962, .T. ) ;
#3271 = CIRCLE ( 'NONE', #10551, 3.000000000000000000 ) ;
#3272 = CARTESIAN_POINT ( 'NONE',  ( -89.14047854185180597, 6.938893903907228378E-15, 100.5765140304660861 ) ) ;
#3273 = DIRECTION ( 'NONE',  ( -0.1566598588826321747, 0.9876526153536343555, 0.000000000000000000 ) ) ;
#3274 = EDGE_CURVE ( 'NONE', #15309, #5835, #1140, .T. ) ;
#3275 = DIRECTION ( 'NONE',  ( -0.9876526153536336894, -0.1566598588826349503, 0.000000000000000000 ) ) ;
#3276 = AXIS2_PLACEMENT_3D ( 'NONE', #6252, #12089, #17937 ) ;
#3277 = EDGE_LOOP ( 'NONE', ( #2347, #7274, #18296, #12313 ) ) ;
#3278 = DIRECTION ( 'NONE',  ( -0.1566598588826321192, 0.9876526153536342445, 7.798540720466731404E-17 ) ) ;
#3279 = CARTESIAN_POINT ( 'NONE',  ( -8.516422466834198346, -21.60064689605303911, 1.522258424776792809E-14 ) ) ;
#3280 = EDGE_LOOP ( 'NONE', ( #13552, #18153, #3167, #1818 ) ) ;
#3282 = VERTEX_POINT ( 'NONE', #7828 ) ;
#3281 = CARTESIAN_POINT ( 'NONE',  ( 0.000000000000000000, 0.000000000000000000, 30.00000000000000000 ) ) ;
#3283 = AXIS2_PLACEMENT_3D ( 'NONE', #3945, #14391, #5584 ) ;
#3284 = ORIENTED_EDGE ( 'NONE', *, *, #4389, .T. ) ;
#3285 = CARTESIAN_POINT ( 'NONE',  ( -129.1404785418517918, -2.850701963179328668, 9.951701414186818625E-16 ) ) ;
#3286 = VECTOR ( 'NONE', #3311, 1000.000000000000000 ) ;
#3287 = VERTEX_POINT ( 'NONE', #7925 ) ;
#3288 = ORIENTED_EDGE ( 'NONE', *, *, #833, .T. ) ;
#3289 = FACE_OUTER_BOUND ( 'NONE', #16223, .T. ) ;
#3290 = AXIS2_PLACEMENT_3D ( 'NONE', #6618, #9353, #13699 ) ;
#3291 = CIRCLE ( 'NONE', #9687, 1.499999999999999556 ) ;
#3292 = VECTOR ( 'NONE', #10736, 1000.000000000000000 ) ;
#3293 = VECTOR ( 'NONE', #7540, 1000.000000000000000 ) ;
#3294 = DIRECTION ( 'NONE',  ( -1.224646799147353207E-16, 1.000000000000000000, 0.000000000000000000 ) ) ;
#3295 = CARTESIAN_POINT ( 'NONE',  ( -76.88766983611584749, -2.536636612185957595, -7.500000000000000000 ) ) ;
#3296 = DIRECTION ( 'NONE',  ( -0.1566598588826321192, 0.9876526153536342445, 7.798540720466731404E-17 ) ) ;
#3297 = AXIS2_PLACEMENT_3D ( 'NONE', #7847, #3903, #14854 ) ;
#3298 = CIRCLE ( 'NONE', #13290, 1.500000000000000444 ) ;
#3299 = ADVANCED_FACE ( 'NONE', ( #3633 ), #16754, .F. ) ;
#3300 = CYLINDRICAL_SURFACE ( 'NONE', #6319, 1.500000000000001554 ) ;
#3301 = DIRECTION ( 'NONE',  ( -0.1566598588826321192, 0.9876526153536342445, 7.798540720466731404E-17 ) ) ;
#3302 = AXIS2_PLACEMENT_3D ( 'NONE', #6486, #13743, #10715 ) ;
#3303 = DIRECTION ( 'NONE',  ( -0.1566598588826321192, 0.9876526153536342445, 7.798540720466730171E-17 ) ) ;
#3304 = CARTESIAN_POINT ( 'NONE',  ( -89.99999999999998579, -35.00000000000001421, 2.500000000000000000 ) ) ;
#3305 = ORIENTED_EDGE ( 'NONE', *, *, #17292, .F. ) ;
#3306 = AXIS2_PLACEMENT_3D ( 'NONE', #5358, #9889, #8002 ) ;
#3307 = CARTESIAN_POINT ( 'NONE',  ( -15.71946376104596155, -17.68067290202200326, 1.908195823574487804E-14 ) ) ;
#3308 = VERTEX_POINT ( 'NONE', #13870 ) ;
#3309 = DIRECTION ( 'NONE',  ( 0.9201637183752249260, 0.3915338189555018777, 0.000000000000000000 ) ) ;
#3310 = EDGE_CURVE ( 'NONE', #2537, #8740, #16558, .T. ) ;
#3311 = DIRECTION ( 'NONE',  ( -0.1566598588826321192, 0.9876526153536342445, 7.798540720466730171E-17 ) ) ;
#3312 = ADVANCED_FACE ( 'NONE', ( #4396 ), #7264, .F. ) ;
#3313 = VERTEX_POINT ( 'NONE', #3068 ) ;
#3314 = CARTESIAN_POINT ( 'NONE',  ( -59.79999999999999716, 0.000000000000000000, -25.00000000000000000 ) ) ;
#3315 = VERTEX_POINT ( 'NONE', #6008 ) ;
#3316 = AXIS2_PLACEMENT_3D ( 'NONE', #741, #11033, #16774 ) ;
#3317 = VERTEX_POINT ( 'NONE', #17602 ) ;
#3318 = DIRECTION ( 'NONE',  ( -0.1566598588826321192, 0.9876526153536342445, 7.798540720466730171E-17 ) ) ;
#3319 = EDGE_LOOP ( 'NONE', ( #12347, #1645, #8615, #17813 ) ) ;
#3320 = AXIS2_PLACEMENT_3D ( 'NONE', #9459, #10958, #1054 ) ;
#3321 = FACE_BOUND ( 'NONE', #360, .T. ) ;
#3322 = AXIS2_PLACEMENT_3D ( 'NONE', #7981, #15189, #10802 ) ;
#3323 = AXIS2_PLACEMENT_3D ( 'NONE', #2320, #12465, #6803 ) ;
#3324 = ORIENTED_EDGE ( 'NONE', *, *, #14007, .T. ) ;
#3325 = ORIENTED_EDGE ( 'NONE', *, *, #15865, .F. ) ;
#3326 = CARTESIAN_POINT ( 'NONE',  ( -70.00000000000000000, 44.99999999999999289, 25.00000000000000000 ) ) ;
#3327 = AXIS2_PLACEMENT_3D ( 'NONE', #16452, #529, #8087 ) ;
#3328 = EDGE_CURVE ( 'NONE', #4041, #15663, #8072, .T. ) ;
#3329 = CARTESIAN_POINT ( 'NONE',  ( -69.54653129781877396, -26.21863521112543438, -4.330127018922180326 ) ) ;
#3331 = CARTESIAN_POINT ( 'NONE',  ( -35.67686938905902849, -25.90879301532540779, -12.99038105676658006 ) ) ;
#3330 = CIRCLE ( 'NONE', #11804, 2.500000000000002220 ) ;
#3333 = ADVANCED_FACE ( 'NONE', ( #16342 ), #6305, .F. ) ;
#3332 = FACE_OUTER_BOUND ( 'NONE', #1526, .T. ) ;
#3334 = CARTESIAN_POINT ( 'NONE',  ( -49.59961335071797350, 37.20051552679458240, -130.3485206753969976 ) ) ;
#3335 = FACE_OUTER_BOUND ( 'NONE', #6010, .T. ) ;
#3336 = ORIENTED_EDGE ( 'NONE', *, *, #2559, .T. ) ;
#3337 = ORIENTED_EDGE ( 'NONE', *, *, #9952, .F. ) ;
#3338 = DIRECTION ( 'NONE',  ( -0.1566598588826321192, 0.9876526153536342445, 7.798540720466730171E-17 ) ) ;
#3339 = CARTESIAN_POINT ( 'NONE',  ( -129.1404785418517918, -2.850701963179328668, 9.951701414186818625E-16 ) ) ;
#3340 = DIRECTION ( 'NONE',  ( 0.000000000000000000, 0.000000000000000000, 1.000000000000000000 ) ) ;
#3341 = AXIS2_PLACEMENT_3D ( 'NONE', #18499, #12548, #932 ) ;
#3342 = ORIENTED_EDGE ( 'NONE', *, *, #7989, .F. ) ;
#3343 = ORIENTED_EDGE ( 'NONE', *, *, #8154, .F. ) ;
#3344 = DIRECTION ( 'NONE',  ( -0.9876526153536344665, -0.1566598588826304539, 0.000000000000000000 ) ) ;
#3345 = AXIS2_PLACEMENT_3D ( 'NONE', #7566, #17538, #8889 ) ;
#3346 = AXIS2_PLACEMENT_3D ( 'NONE', #12462, #6513, #8306 ) ;
#3347 = EDGE_CURVE ( 'NONE', #8246, #18620, #6901, .T. ) ;
#3348 = VECTOR ( 'NONE', #11570, 1000.000000000000000 ) ;
#3349 = CARTESIAN_POINT ( 'NONE',  ( -7.818242838216901802, -16.42739403096095074, 17.32050807568881012 ) ) ;
#3350 = EDGE_CURVE ( 'NONE', #4040, #1622, #11071, .T. ) ;
#3351 = ORIENTED_EDGE ( 'NONE', *, *, #5236, .T. ) ;
#3352 = ADVANCED_FACE ( 'NONE', ( #3335 ), #12505, .F. ) ;
#3353 = EDGE_CURVE ( 'NONE', #15259, #1477, #9887, .T. ) ;
#3354 = DIRECTION ( 'NONE',  ( -0.9876526153536341335, -0.1566598588826327021, 0.000000000000000000 ) ) ;
#3355 = CARTESIAN_POINT ( 'NONE',  ( -86.18478963674542115, 32.34879426031891114, -30.00000000000000355 ) ) ;
#3356 = VECTOR ( 'NONE', #5869, 1000.000000000000000 ) ;
#3357 = AXIS2_PLACEMENT_3D ( 'NONE', #8174, #14036, #12600 ) ;
#3358 = DIRECTION ( 'NONE',  ( -0.9876526153536336894, -0.1566598588826349503, 0.000000000000000000 ) ) ;
#3359 = VERTEX_POINT ( 'NONE', #3236 ) ;
#3360 = ORIENTED_EDGE ( 'NONE', *, *, #15572, .F. ) ;
#3361 = FACE_OUTER_BOUND ( 'NONE', #2587, .T. ) ;
#3362 = ORIENTED_EDGE ( 'NONE', *, *, #18484, .T. ) ;
#3363 = CIRCLE ( 'NONE', #18564, 1.499999999999999556 ) ;
#3364 = VERTEX_POINT ( 'NONE', #9034 ) ;
#3365 = AXIS2_PLACEMENT_3D ( 'NONE', #3054, #11477, #14434 ) ;
#3366 = DIRECTION ( 'NONE',  ( -0.9876526153536344665, -0.1566598588826304539, 0.000000000000000000 ) ) ;
#3367 = AXIS2_PLACEMENT_3D ( 'NONE', #14884, #17386, #17468 ) ;
#3368 = CARTESIAN_POINT ( 'NONE',  ( -90.00000000000000000, 34.99999999999999289, 100.5765140304660861 ) ) ;
#3369 = ORIENTED_EDGE ( 'NONE', *, *, #6000, .T. ) ;
#3370 = CARTESIAN_POINT ( 'NONE',  ( -35.67686938905904270, -25.90879301532540779, -21.65063509461098334 ) ) ;
#3371 = CARTESIAN_POINT ( 'NONE',  ( -9.464440072009985272, -79.45648819128378193, 17.32050807568880657 ) ) ;
#3372 = CARTESIAN_POINT ( 'NONE',  ( -76.17062661855784711, -32.33184722951329348, 8.660254037844417496 ) ) ;
#3373 = CARTESIAN_POINT ( 'NONE',  ( -3.044698072211382112, -78.43819910854666944, 8.660254037844408614 ) ) ;
#3374 = CYLINDRICAL_SURFACE ( 'NONE', #18458, 1.500000000000001554 ) ;
#3375 = CARTESIAN_POINT ( 'NONE',  ( -20.32861884089991023, -81.17974663899272514, 4.330127018922213189 ) ) ;
#3377 = ORIENTED_EDGE ( 'NONE', *, *, #16026, .F. ) ;
#3376 = CARTESIAN_POINT ( 'NONE',  ( 2.000000000000000000, 0.000000000000000000, -20.00000000000000355 ) ) ;
#3378 = EDGE_CURVE ( 'NONE', #18416, #16068, #325, .T. ) ;
#3379 = CIRCLE ( 'NONE', #8259, 1.500000000000000000 ) ;
#3380 = EDGE_CURVE ( 'NONE', #12090, #3317, #18738, .T. ) ;
#3381 = CARTESIAN_POINT ( 'NONE',  ( -23.33121169713865584, -23.95054477929251036, 1.869203119972154228E-14 ) ) ;
#3382 = VERTEX_POINT ( 'NONE', #9309 ) ;
#3383 = EDGE_LOOP ( 'NONE', ( #13747, #12542 ) ) ;
#3384 = LINE ( 'NONE', #11819, #1432 ) ;
#3385 = CIRCLE ( 'NONE', #10019, 1.500000000000000888 ) ;
#3386 = CYLINDRICAL_SURFACE ( 'NONE', #7042, 1.500000000000000888 ) ;
#3387 = LINE ( 'NONE', #8910, #7965 ) ;
#3388 = LINE ( 'NONE', #18242, #1544 ) ;
#3389 = LINE ( 'NONE', #12291, #6432 ) ;
#3390 = PRODUCT_DEFINITION_CONTEXT ( 'detailed design', #12682, 'design' ) ;
#3391 = CARTESIAN_POINT ( 'NONE',  ( -129.0554062880559343, -14.67359210495141575, -4.766626691765363688 ) ) ;
#3392 = LINE ( 'NONE', #9198, #11128 ) ;
#3393 = CARTESIAN_POINT ( 'NONE',  ( -67.07739975943471222, -25.82698556391886413, 17.32050807568881723 ) ) ;
#3394 = DIRECTION ( 'NONE',  ( -0.1566598588826321192, 0.9876526153536342445, 7.798540720466730171E-17 ) ) ;
#3395 = CARTESIAN_POINT ( 'NONE',  ( -44.03228160938703439, -84.93958325217590755, 1.424741226644455312E-14 ) ) ;
#3396 = VERTEX_POINT ( 'NONE', #3424 ) ;
#3397 = CARTESIAN_POINT ( 'NONE',  ( -129.1404785418517918, -2.850701963179328668, 9.951701414186818625E-16 ) ) ;
#3398 = ORIENTED_EDGE ( 'NONE', *, *, #18359, .F. ) ;
#3399 = AXIS2_PLACEMENT_3D ( 'NONE', #12884, #8824, #16023 ) ;
#3400 = DIRECTION ( 'NONE',  ( -0.000000000000000000, -0.000000000000000000, -1.000000000000000000 ) ) ;
#3401 = DIRECTION ( 'NONE',  ( -0.1566598588826321192, 0.9876526153536342445, 7.798540720466730171E-17 ) ) ;
#3402 = LINE ( 'NONE', #16136, #18791 ) ;
#3403 = ADVANCED_FACE ( 'NONE', ( #16897 ), #6751, .F. ) ;
#3404 = ORIENTED_EDGE ( 'NONE', *, *, #2406, .T. ) ;
#3405 = ORIENTED_EDGE ( 'NONE', *, *, #2081, .F. ) ;
#3406 = ORIENTED_EDGE ( 'NONE', *, *, #978, .F. ) ;
#3407 = ORIENTED_EDGE ( 'NONE', *, *, #13160, .F. ) ;
#3408 = DIRECTION ( 'NONE',  ( -0.1566598588826321192, 0.9876526153536342445, 7.798540720466731404E-17 ) ) ;
#3409 = EDGE_CURVE ( 'NONE', #12681, #1415, #13291, .T. ) ;
#3410 = ORIENTED_EDGE ( 'NONE', *, *, #3122, .F. ) ;
#3411 = FACE_BOUND ( 'NONE', #14343, .T. ) ;
#3412 = ORIENTED_EDGE ( 'NONE', *, *, #15297, .T. ) ;
#3413 = TOROIDAL_SURFACE ( 'NONE', #5868, 12.83663829214476770, 3.000000000000000000 ) ;
#3414 = CYLINDRICAL_SURFACE ( 'NONE', #14310, 1.500000000000001554 ) ;
#3415 = EDGE_LOOP ( 'NONE', ( #4201, #12118, #18417, #14824 ) ) ;
#3416 = EDGE_CURVE ( 'NONE', #14596, #18395, #11106, .T. ) ;
#3417 = ORIENTED_EDGE ( 'NONE', *, *, #8627, .F. ) ;
#3418 = CARTESIAN_POINT ( 'NONE',  ( -38.92930022185625205, -21.36217958576385456, 8.660254037844417496 ) ) ;
#3419 = ORIENTED_EDGE ( 'NONE', *, *, #13997, .F. ) ;
#3420 = CARTESIAN_POINT ( 'NONE',  ( -89.99999999999998579, -35.00000000000001421, 30.00000000000002487 ) ) ;
#3421 = DIRECTION ( 'NONE',  ( -0.9876526153536341335, -0.1566598588826327021, 0.000000000000000000 ) ) ;
#3422 = CARTESIAN_POINT ( 'NONE',  ( -71.02801022084922522, -26.45362499944938861, 21.65063509461102242 ) ) ;
#3423 = DIRECTION ( 'NONE',  ( -0.1566598588826321747, 0.9876526153536343555, 0.000000000000000000 ) ) ;
#3424 = CARTESIAN_POINT ( 'NONE',  ( -79.50968810220766159, 31.87664632526870889, 30.00000000000002842 ) ) ;
#3425 = VERTEX_POINT ( 'NONE', #7804 ) ;
#3426 = EDGE_LOOP ( 'NONE', ( #14987, #10223 ) ) ;
#3427 = CARTESIAN_POINT ( 'NONE',  ( 55.85952145814821534, 6.938893903907228378E-15, 2.500000000000000000 ) ) ;
#3428 = CYLINDRICAL_SURFACE ( 'NONE', #16355, 1.500000000000001554 ) ;
#3429 = DIRECTION ( 'NONE',  ( -0.9826218788918641422, -0.1856185419698762606, 0.000000000000000000 ) ) ;
#3430 = EDGE_CURVE ( 'NONE', #16818, #6018, #8993, .T. ) ;
#3431 = ORIENTED_EDGE ( 'NONE', *, *, #12952, .T. ) ;
#3432 = DIRECTION ( 'NONE',  ( 2.273171532858076093E-17, -1.203364738757079611E-16, 1.000000000000000000 ) ) ;
#3433 = ORIENTED_EDGE ( 'NONE', *, *, #3792, .T. ) ;
#3434 = ADVANCED_FACE ( 'NONE', ( #7901 ), #10506, .T. ) ;
#3435 = CARTESIAN_POINT ( 'NONE',  ( -79.50968810220766159, 31.87664632526870889, -35.00000000000000000 ) ) ;
#3436 = CYLINDRICAL_SURFACE ( 'NONE', #5441, 1.500000000000001554 ) ;
#3437 = CARTESIAN_POINT ( 'NONE',  ( -21.64537945316773460, -18.62063205531779531, -12.99038105676658006 ) ) ;
#3438 = DIRECTION ( 'NONE',  ( -0.9826218788918642533, -0.1856185419698762884, 0.000000000000000000 ) ) ;
#3439 = CARTESIAN_POINT ( 'NONE',  ( 73.09088021254186174, 1.387778780781445676E-14, -19.99999999999999645 ) ) ;
#3440 = VERTEX_POINT ( 'NONE', #10449 ) ;
#3441 = CYLINDRICAL_SURFACE ( 'NONE', #8641, 1.500000000000001554 ) ;
#3442 = VERTEX_POINT ( 'NONE', #6944 ) ;
#3443 = EDGE_LOOP ( 'NONE', ( #7347, #604, #4068, #11841 ) ) ;
#3444 = CARTESIAN_POINT ( 'NONE',  ( -61.84966369593024638, -30.06027927571514624, 4.330127018922217630 ) ) ;
#3445 = ORIENTED_EDGE ( 'NONE', *, *, #150, .F. ) ;
#3446 = ORIENTED_EDGE ( 'NONE', *, *, #13764, .F. ) ;
#3447 = ORIENTED_EDGE ( 'NONE', *, *, #4114, .F. ) ;
#3448 = EDGE_CURVE ( 'NONE', #12256, #14889, #11267, .T. ) ;
#3449 = EDGE_CURVE ( 'NONE', #18006, #1662, #7044, .T. ) ;
#3450 = EDGE_CURVE ( 'NONE', #898, #4657, #5602, .T. ) ;
#3451 = AXIS2_PLACEMENT_3D ( 'NONE', #9482, #2184, #6556 ) ;
#3452 = CARTESIAN_POINT ( 'NONE',  ( -61.31620237807555895, -87.68113078262194904, -4.330127018922185655 ) ) ;
#3453 = EDGE_CURVE ( 'NONE', #14006, #14647, #218, .T. ) ;
#3454 = DIRECTION ( 'NONE',  ( -0.1566598588826321747, 0.9876526153536343555, 0.000000000000000000 ) ) ;
#3455 = ADVANCED_FACE ( 'NONE', ( #5084 ), #9360, .F. ) ;
#3456 = CYLINDRICAL_SURFACE ( 'NONE', #10978, 150.0000000000000284 ) ;
#3457 = CARTESIAN_POINT ( 'NONE',  ( -172.7326993491721225, 43.83249341393818810, 9.951701414186830458E-16 ) ) ;
#3458 = DIRECTION ( 'NONE',  ( -0.9876526153536341335, -0.1566598588826327021, 0.000000000000000000 ) ) ;
#3459 = PRODUCT_RELATED_PRODUCT_CATEGORY ( 'part', '', ( #3936 ) ) ;
#3460 = PRODUCT_DEFINITION_SHAPE ( 'NONE', 'NONE',  #12765 ) ;
#3461 = CARTESIAN_POINT ( 'NONE',  ( -20.86208015875457988, -23.55889513208593655, -21.65063509461098334 ) ) ;
#3462 = CARTESIAN_POINT ( 'NONE',  ( -23.12685837619818940, -18.85562184364174598, 12.99038105676661736 ) ) ;
#3463 = DIRECTION ( 'NONE',  ( -0.9876526153536336894, -0.1566598588826349503, 0.000000000000000000 ) ) ;
#3464 = FACE_OUTER_BOUND ( 'NONE', #11568, .T. ) ;
#3465 = AXIS2_PLACEMENT_3D ( 'NONE', #4100, #11216, #9525 ) ;
#3466 = DIRECTION ( 'NONE',  ( -0.1566598588826321192, 0.9876526153536342445, 7.798540720466730171E-17 ) ) ;
#3468 = VERTEX_POINT ( 'NONE', #847 ) ;
#3467 = DIRECTION ( 'NONE',  ( 0.000000000000000000, 0.000000000000000000, 1.000000000000000000 ) ) ;
#3469 = CARTESIAN_POINT ( 'NONE',  ( -75.18297400320422241, -32.17518737063066681, -12.99038105676658006 ) ) ;
#3470 = VERTEX_POINT ( 'NONE', #12382 ) ;
#3471 = ORIENTED_EDGE ( 'NONE', *, *, #16638, .T. ) ;
#3472 = ADVANCED_FACE ( 'NONE', ( #6354 ), #10595, .F. ) ;
#3473 = VERTEX_POINT ( 'NONE', #18022 ) ;
#3474 = CARTESIAN_POINT ( 'NONE',  ( -21.81009776393036503, -81.41473642731669713, 12.99038105676661203 ) ) ;
#3475 = ADVANCED_FACE ( 'NONE', ( #16482 ), #9552, .F. ) ;
#3476 = CARTESIAN_POINT ( 'NONE',  ( -35.14340807120436239, -83.52964452223220349, -12.99038105676658539 ) ) ;
#3477 = CIRCLE ( 'NONE', #5929, 1.500000000000000888 ) ;
#3478 = PRODUCT_RELATED_PRODUCT_CATEGORY ( 'part', '', ( #9076 ) ) ;
#3479 = CARTESIAN_POINT ( 'NONE',  ( 5.350349158294472218, -77.10659030804430358, 17.32050807568880657 ) ) ;
#3480 = DIRECTION ( 'NONE',  ( -0.9876526153536336894, -0.1566598588826349503, 0.000000000000000000 ) ) ;
#3481 = EDGE_CURVE ( 'NONE', #311, #14160, #11996, .T. ) ;
#3482 = EDGE_CURVE ( 'NONE', #7247, #7443, #11423, .T. ) ;
#3483 = DIRECTION ( 'NONE',  ( -0.1566598588826321192, 0.9876526153536342445, 7.798540720466730171E-17 ) ) ;
#3484 = DIRECTION ( 'NONE',  ( 0.000000000000000000, 0.000000000000000000, 1.000000000000000000 ) ) ;
#3485 = ORIENTED_EDGE ( 'NONE', *, *, #10745, .F. ) ;
#3486 = DIRECTION ( 'NONE',  ( -0.9876526153536336894, -0.1566598588826349503, 0.000000000000000000 ) ) ;
#3487 = ORIENTED_EDGE ( 'NONE', *, *, #17924, .F. ) ;
#3488 = FACE_BOUND ( 'NONE', #2050, .T. ) ;
#3489 = SURFACE_STYLE_USAGE ( .BOTH. , #16499 ) ;
#3490 = CARTESIAN_POINT ( 'NONE',  ( -309.1404785418517918, -2.850701963179326892, -12.83663829214475882 ) ) ;
#3491 = CARTESIAN_POINT ( 'NONE',  ( -58.88670584986932965, -29.59029969906724844, -21.65063509461098334 ) ) ;
#3492 = ORIENTED_EDGE ( 'NONE', *, *, #7729, .F. ) ;
#3493 = AXIS2_PLACEMENT_3D ( 'NONE', #12500, #5312, #12581 ) ;
#3494 = VERTEX_POINT ( 'NONE', #2823 ) ;
#3495 = ORIENTED_EDGE ( 'NONE', *, *, #10445, .T. ) ;
#3496 = ORIENTED_EDGE ( 'NONE', *, *, #6088, .T. ) ;
#3497 = DIRECTION ( 'NONE',  ( -0.9876526153536336894, -0.1566598588826350336, 0.000000000000000000 ) ) ;
#3498 = FACE_BOUND ( 'NONE', #6231, .T. ) ;
#3499 = AXIS2_PLACEMENT_3D ( 'NONE', #17963, #4742, #9119 ) ;
#3500 = DIRECTION ( 'NONE',  ( -0.1566598588826321747, 0.9876526153536343555, 0.000000000000000000 ) ) ;
#3501 = VERTEX_POINT ( 'NONE', #12563 ) ;
#3502 = EDGE_CURVE ( 'NONE', #9820, #17699, #18451, .T. ) ;
#3503 = AXIS2_PLACEMENT_3D ( 'NONE', #5196, #3743, #9547 ) ;
#3504 = EDGE_CURVE ( 'NONE', #1028, #5886, #2043, .T. ) ;
#3505 = CARTESIAN_POINT ( 'NONE',  ( -50.49165861936349131, -28.25869089856488614, -21.65063509461098334 ) ) ;
#3506 = EDGE_LOOP ( 'NONE', ( #10567, #5841, #17066, #12591 ) ) ;
#3507 = CARTESIAN_POINT ( 'NONE',  ( 0.5768043922889515285, -15.09578523045857601, 8.660254037844412167 ) ) ;
#3508 = DIRECTION ( 'NONE',  ( 0.000000000000000000, 0.000000000000000000, 1.000000000000000000 ) ) ;
#3509 = CYLINDRICAL_SURFACE ( 'NONE', #10443, 2.199999999999993516 ) ;
#3510 = TOROIDAL_SURFACE ( 'NONE', #12607, 13.78215425775057668, 2.000000000000000000 ) ;
#3511 = ORIENTED_EDGE ( 'NONE', *, *, #17053, .T. ) ;
#3512 = ORIENTED_EDGE ( 'NONE', *, *, #9056, .T. ) ;
#3513 = DIRECTION ( 'NONE',  ( 0.000000000000000000, 0.000000000000000000, 1.000000000000000000 ) ) ;
#3514 = CIRCLE ( 'NONE', #513, 1.500000000000000444 ) ;
#3515 = LINE ( 'NONE', #14725, #16581 ) ;
#3516 = EDGE_LOOP ( 'NONE', ( #17717, #16519, #12790, #7153 ) ) ;
#3517 = ORIENTED_EDGE ( 'NONE', *, *, #8216, .T. ) ;
#3518 = CIRCLE ( 'NONE', #18723, 1.500000000000001332 ) ;
#3519 = ORIENTED_EDGE ( 'NONE', *, *, #12303, .F. ) ;
#3520 = VERTEX_POINT ( 'NONE', #11247 ) ;
#3521 = DIRECTION ( 'NONE',  ( 0.9876526153536342445, 0.1566598588826321470, 6.424890667364402638E-17 ) ) ;
#3522 = CIRCLE ( 'NONE', #14135, 1.500000000000000888 ) ;
#3523 = DIRECTION ( 'NONE',  ( -0.9876526153536341335, -0.1566598588826327021, 0.000000000000000000 ) ) ;
#3524 = VECTOR ( 'NONE', #10270, 1000.000000000000000 ) ;
#3525 = DIRECTION ( 'NONE',  ( -0.9998476951563911586, -2.137303368083795934E-18, 0.01745240643728354635 ) ) ;
#3526 = DIRECTION ( 'NONE',  ( -0.1566598588826321192, 0.9876526153536342445, 7.798540720466731404E-17 ) ) ;
#3527 = DIRECTION ( 'NONE',  ( -0.9876526153536341335, -0.1566598588826327021, 0.000000000000000000 ) ) ;
#3528 = EDGE_CURVE ( 'NONE', #9211, #17125, #2338, .T. ) ;
#3529 = CARTESIAN_POINT ( 'NONE',  ( -51.43967622453925514, -86.11453219379563961, 12.99038105676661203 ) ) ;
#3530 = DIRECTION ( 'NONE',  ( -0.000000000000000000, -0.000000000000000000, -1.000000000000000000 ) ) ;
#3531 = ORIENTED_EDGE ( 'NONE', *, *, #708, .T. ) ;
#3532 = CIRCLE ( 'NONE', #9608, 1.500000000000001332 ) ;
#3533 = DIRECTION ( 'NONE',  ( -0.1566598588826321747, 0.9876526153536343555, 0.000000000000000000 ) ) ;
#3534 = DIRECTION ( 'NONE',  ( 0.000000000000000000, 0.000000000000000000, 1.000000000000000000 ) ) ;
#3535 = CARTESIAN_POINT ( 'NONE',  ( -6.830590222863280658, -16.27073417207831696, -21.65063509461097979 ) ) ;
#3536 = ORIENTED_EDGE ( 'NONE', *, *, #3774, .T. ) ;
#3537 = ORIENTED_EDGE ( 'NONE', *, *, #18192, .T. ) ;
#3538 = FACE_OUTER_BOUND ( 'NONE', #16194, .T. ) ;
#3539 = ORIENTED_EDGE ( 'NONE', *, *, #7966, .F. ) ;
#3540 = EDGE_CURVE ( 'NONE', #10934, #11092, #11051, .T. ) ;
#3541 = CARTESIAN_POINT ( 'NONE',  ( -21.81009776393036503, -81.41473642731669713, 12.99038105676661203 ) ) ;
#3542 = ORIENTED_EDGE ( 'NONE', *, *, #10944, .T. ) ;
#3543 = EDGE_LOOP ( 'NONE', ( #7602, #3069 ) ) ;
#3544 = DIRECTION ( 'NONE',  ( -0.1566598588826321192, 0.9876526153536342445, 7.798540720466731404E-17 ) ) ;
#3545 = AXIS2_PLACEMENT_3D ( 'NONE', #9200, #7774, #12201 ) ;
#3546 = CARTESIAN_POINT ( 'NONE',  ( -37.44782129882580080, -21.12718979743991099, 8.660254037844417496 ) ) ;
#3547 = DIRECTION ( 'NONE',  ( 0.000000000000000000, 0.000000000000000000, -1.000000000000000000 ) ) ;
#3548 = LINE ( 'NONE', #3737, #1346 ) ;
#3549 = ORIENTED_EDGE ( 'NONE', *, *, #6813, .F. ) ;
#3550 = DIRECTION ( 'NONE',  ( -0.1566598588826321192, 0.9876526153536342445, 7.798540720466730171E-17 ) ) ;
#3551 = CARTESIAN_POINT ( 'NONE',  ( -55.22556837519114481, -23.94706725732728003, 17.32050807568881723 ) ) ;
#3552 = CIRCLE ( 'NONE', #2669, 1.500000000000001332 ) ;
#3553 = CARTESIAN_POINT ( 'NONE',  ( -11.97320662057189899, -22.14895640214223960, 1.887572821959364500E-14 ) ) ;
#3555 = FACE_OUTER_BOUND ( 'NONE', #8307, .T. ) ;
#3554 = AXIS2_PLACEMENT_3D ( 'NONE', #11191, #9312, #11093 ) ;
#3556 = EDGE_CURVE ( 'NONE', #11687, #4660, #15055, .T. ) ;
#3557 = AXIS2_PLACEMENT_3D ( 'NONE', #4916, #6548, #18039 ) ;
#3558 = DIRECTION ( 'NONE',  ( 1.000000000000000000, 0.000000000000000000, 0.000000000000000000 ) ) ;
#3559 = CIRCLE ( 'NONE', #9325, 1.500000000000000888 ) ;
#3560 = DIRECTION ( 'NONE',  ( -0.9876526153536341335, -0.1566598588826327021, 0.000000000000000000 ) ) ;
#3561 = EDGE_CURVE ( 'NONE', #10291, #16721, #11039, .T. ) ;
#3563 = VERTEX_POINT ( 'NONE', #15430 ) ;
#3562 = CARTESIAN_POINT ( 'NONE',  ( -41.39843176024034221, -21.75382923297042481, -12.99038105676658006 ) ) ;
#3564 = EDGE_CURVE ( 'NONE', #1595, #2455, #2451, .T. ) ;
#3565 = CARTESIAN_POINT ( 'NONE',  ( -4.526176995241833367, -78.67318889687062722, 1.424741226644455312E-14 ) ) ;
#3566 = ORIENTED_EDGE ( 'NONE', *, *, #18340, .F. ) ;
#3567 = ORIENTED_EDGE ( 'NONE', *, *, #4933, .F. ) ;
#3568 = AXIS2_PLACEMENT_3D ( 'NONE', #15277, #6774, #3886 ) ;
#3569 = LINE ( 'NONE', #13712, #4281 ) ;
#3570 = AXIS2_PLACEMENT_3D ( 'NONE', #16568, #9077, #841 ) ;
#3571 = CARTESIAN_POINT ( 'NONE',  ( -312.1404785418517918, -2.850701963179328668, 15.88900348692940945 ) ) ;
#3572 = DIRECTION ( 'NONE',  ( -0.000000000000000000, -0.000000000000000000, -1.000000000000000000 ) ) ;
#3573 = UNCERTAINTY_MEASURE_WITH_UNIT (LENGTH_MEASURE( 1.000000000000000082E-05 ), #744, 'distance_accuracy_value', 'NONE');
#3574 = FACE_OUTER_BOUND ( 'NONE', #6085, .T. ) ;
#3575 = DIRECTION ( 'NONE',  ( -0.1566598588826321192, 0.9876526153536342445, 7.798540720466730171E-17 ) ) ;
#3576 = ORIENTED_EDGE ( 'NONE', *, *, #9854, .F. ) ;
#3577 = CARTESIAN_POINT ( 'NONE',  ( -28.06512145296634486, -19.63892113805490780, 12.99038105676661736 ) ) ;
#3578 = EDGE_CURVE ( 'NONE', #3908, #16065, #6299, .T. ) ;
#3579 = ORIENTED_EDGE ( 'NONE', *, *, #18601, .T. ) ;
#3580 = CIRCLE ( 'NONE', #6632, 1.499999999999999556 ) ;
#3581 = EDGE_CURVE ( 'NONE', #16919, #13271, #5387, .T. ) ;
#3582 = CARTESIAN_POINT ( 'NONE',  ( -29.21749237908258223, -82.58968536893641499, -8.660254037844385522 ) ) ;
#3583 = DIRECTION ( 'NONE',  ( -0.1566598588826321192, 0.9876526153536342445, 7.798540720466731404E-17 ) ) ;
#3584 = CARTESIAN_POINT ( 'NONE',  ( -25.10216360690543524, -19.16894156140700289, -21.65063509461098334 ) ) ;
#3585 = VECTOR ( 'NONE', #3130, 1000.000000000000000 ) ;
#3586 = VECTOR ( 'NONE', #14652, 1000.000000000000000 ) ;
#3587 = FACE_OUTER_BOUND ( 'NONE', #16613, .T. ) ;
#3588 = CIRCLE ( 'NONE', #14205, 1.500000000000000888 ) ;
#3589 = VECTOR ( 'NONE', #13239, 1000.000000000000000 ) ;
#3590 = VERTEX_POINT ( 'NONE', #1235 ) ;
#3591 = VERTEX_POINT ( 'NONE', #3943 ) ;
#3592 = EDGE_LOOP ( 'NONE', ( #8832, #3938 ) ) ;
#3593 = CARTESIAN_POINT ( 'NONE',  ( 2.200000000000000178, 2.694222958124177006E-16, -25.00000000000000000 ) ) ;
#3594 = FACE_BOUND ( 'NONE', #188, .T. ) ;
#3595 = VECTOR ( 'NONE', #15570, 1000.000000000000000 ) ;
#3596 = CARTESIAN_POINT ( 'NONE',  ( -69.54653129781877396, -26.21863521112542728, -21.65063509461098334 ) ) ;
#3597 = AXIS2_PLACEMENT_3D ( 'NONE', #11931, #9218, #7801 ) ;
#3598 = ORIENTED_EDGE ( 'NONE', *, *, #13598, .T. ) ;
#3599 = CIRCLE ( 'NONE', #17283, 1.500000000000000444 ) ;
#3600 = AXIS2_PLACEMENT_3D ( 'NONE', #772, #5225, #2269 ) ;
#3601 = CARTESIAN_POINT ( 'NONE',  ( -126.1404785418517918, 9.595891400605990995, 2.500000000000000000 ) ) ;
#3602 = VERTEX_POINT ( 'NONE', #12766 ) ;
#3603 = LINE ( 'NONE', #9413, #11476 ) ;
#3604 = CIRCLE ( 'NONE', #5762, 1.500000000000001332 ) ;
#3605 = DIRECTION ( 'NONE',  ( -0.1566598588826321192, 0.9876526153536342445, 7.798540720466730171E-17 ) ) ;
#3606 = ORIENTED_EDGE ( 'NONE', *, *, #11384, .T. ) ;
#3607 = ORIENTED_EDGE ( 'NONE', *, *, #9925, .T. ) ;
#3608 = CARTESIAN_POINT ( 'NONE',  ( -29.75095369693726610, -24.96883386202961574, 17.32050807568881723 ) ) ;
#3609 = AXIS2_PLACEMENT_3D ( 'NONE', #7340, #16395, #3560 ) ;
#3610 = EDGE_CURVE ( 'NONE', #9493, #18706, #3154, .T. ) ;
#3611 = DIRECTION ( 'NONE',  ( 0.000000000000000000, 0.000000000000000000, 1.000000000000000000 ) ) ;
#3612 = ORIENTED_EDGE ( 'NONE', *, *, #2540, .F. ) ;
#3613 = CIRCLE ( 'NONE', #13925, 145.0000000000000284 ) ;
#3614 = LINE ( 'NONE', #12527, #11561 ) ;
#3615 = EDGE_CURVE ( 'NONE', #3470, #13701, #17508, .T. ) ;
#3616 = CONICAL_SURFACE ( 'NONE', #14826, 12.74754878398196567, 0.01745329251994333364 ) ;
#3617 = CARTESIAN_POINT ( 'NONE',  ( -6.047290928450125946, -21.20899724884646531, 21.65063509461101177 ) ) ;
#3618 = LINE ( 'NONE', #8293, #12365 ) ;
#3619 = EDGE_CURVE ( 'NONE', #11326, #3894, #1170, .T. ) ;
#3620 = DIRECTION ( 'NONE',  ( -0.1566598588826321192, 0.9876526153536342445, 7.798540720466730171E-17 ) ) ;
#3621 = CIRCLE ( 'NONE', #7004, 1.499999999999999556 ) ;
#3622 = LINE ( 'NONE', #9430, #3293 ) ;
#3623 = CARTESIAN_POINT ( 'NONE',  ( -6.047290928450125946, -21.20899724884646531, -4.330127018922184767 ) ) ;
#3624 = DIRECTION ( 'NONE',  ( 1.000000000000000000, 0.000000000000000000, 0.000000000000000000 ) ) ;
#3625 = EDGE_LOOP ( 'NONE', ( #5272, #13445, #10394, #10220 ) ) ;
#3626 = AXIS2_PLACEMENT_3D ( 'NONE', #14421, #4178, #2940 ) ;
#3627 = DIRECTION ( 'NONE',  ( -0.1566598588826321192, 0.9876526153536342445, 7.798540720466731404E-17 ) ) ;
#3628 = AXIS2_PLACEMENT_3D ( 'NONE', #3791, #14043, #15375 ) ;
#3629 = PLANE ( 'NONE',  #8081 ) ;
#3630 = EDGE_LOOP ( 'NONE', ( #14623, #14621 ) ) ;
#3631 = DIRECTION ( 'NONE',  ( 0.000000000000000000, 0.000000000000000000, 1.000000000000000000 ) ) ;
#3632 = DIRECTION ( 'NONE',  ( -0.1566598588826321192, 0.9876526153536342445, 7.798540720466731404E-17 ) ) ;
#3633 = FACE_OUTER_BOUND ( 'NONE', #4984, .T. ) ;
#3634 = ORIENTED_EDGE ( 'NONE', *, *, #2033, .T. ) ;
#3635 = VERTEX_POINT ( 'NONE', #58 ) ;
#3636 = DIRECTION ( 'NONE',  ( 0.000000000000000000, 0.000000000000000000, 1.000000000000000000 ) ) ;
#3637 = ORIENTED_EDGE ( 'NONE', *, *, #4750, .T. ) ;
#3638 = ORIENTED_EDGE ( 'NONE', *, *, #14918, .F. ) ;
#3639 = VECTOR ( 'NONE', #12366, 1000.000000000000000 ) ;
#3640 = EDGE_LOOP ( 'NONE', ( #15065, #6815 ) ) ;
#3641 = VERTEX_POINT ( 'NONE', #7439 ) ;
#3642 = CIRCLE ( 'NONE', #321, 1.499999999999999556 ) ;
#3643 = ORIENTED_EDGE ( 'NONE', *, *, #5698, .T. ) ;
#3644 = ORIENTED_EDGE ( 'NONE', *, *, #3220, .F. ) ;
#3645 = EDGE_CURVE ( 'NONE', #16215, #5645, #1157, .T. ) ;
#3646 = DIRECTION ( 'NONE',  ( -0.1566598588826321192, 0.9876526153536342445, 7.798540720466730171E-17 ) ) ;
#3647 = DIRECTION ( 'NONE',  ( -0.9876526153536336894, -0.1566598588826349503, 0.000000000000000000 ) ) ;
#3648 = VECTOR ( 'NONE', #18073, 1000.000000000000000 ) ;
#3649 = CARTESIAN_POINT ( 'NONE',  ( -68.72359699322777260, -88.85607972424168111, 1.424741226644455312E-14 ) ) ;
#3650 = DIRECTION ( 'NONE',  ( -0.1566598588826321192, 0.9876526153536342445, 7.798540720466730171E-17 ) ) ;
#3651 = VERTEX_POINT ( 'NONE', #11668 ) ;
#3652 = DIRECTION ( 'NONE',  ( 0.000000000000000000, 0.000000000000000000, 1.000000000000000000 ) ) ;
#3653 = EDGE_CURVE ( 'NONE', #10352, #4467, #15875, .T. ) ;
#3654 = DIRECTION ( 'NONE',  ( 0.000000000000000000, 0.000000000000000000, 1.000000000000000000 ) ) ;
#3655 = FACE_OUTER_BOUND ( 'NONE', #6658, .T. ) ;
#3656 = FACE_BOUND ( 'NONE', #10064, .T. ) ;
#3657 = DIRECTION ( 'NONE',  ( -0.1566598588826321192, 0.9876526153536342445, 7.798540720466730171E-17 ) ) ;
#3658 = ORIENTED_EDGE ( 'NONE', *, *, #17731, .F. ) ;
#3659 = CIRCLE ( 'NONE', #7916, 1.500000000000000888 ) ;
#3660 = LINE ( 'NONE', #11048, #9401 ) ;
#3661 = ORIENTED_EDGE ( 'NONE', *, *, #10209, .T. ) ;
#3662 = AXIS2_PLACEMENT_3D ( 'NONE', #12821, #5908, #17400 ) ;
#3663 = CARTESIAN_POINT ( 'NONE',  ( -69.99999999999998579, -45.00000000000000711, 25.00000000000000000 ) ) ;
#3664 = DIRECTION ( 'NONE',  ( 0.000000000000000000, 0.000000000000000000, 1.000000000000000000 ) ) ;
#3665 = VERTEX_POINT ( 'NONE', #13200 ) ;
#3666 = ORIENTED_EDGE ( 'NONE', *, *, #5090, .F. ) ;
#3667 = AXIS2_PLACEMENT_3D ( 'NONE', #12424, #11184, #10992 ) ;
#3668 = EDGE_CURVE ( 'NONE', #18393, #730, #1744, .T. ) ;
#3669 = DIRECTION ( 'NONE',  ( -0.9826218788918641422, -0.1856185419698762606, 0.000000000000000000 ) ) ;
#3670 = ORIENTED_EDGE ( 'NONE', *, *, #3481, .T. ) ;
#3671 = CIRCLE ( 'NONE', #6127, 5.000000000000004441 ) ;
#3672 = CARTESIAN_POINT ( 'NONE',  ( -34.97868976044173195, -20.73554015023333719, 21.65063509461101887 ) ) ;
#3673 = CARTESIAN_POINT ( 'NONE',  ( -42.09661138885763876, -26.92708209806250608, -12.99038105676658006 ) ) ;
#3674 = DIRECTION ( 'NONE',  ( -0.3915338189555019333, 0.9201637183752250371, 0.000000000000000000 ) ) ;
#3675 = DIRECTION ( 'NONE',  ( 0.000000000000000000, 0.000000000000000000, 1.000000000000000000 ) ) ;
#3676 = EDGE_CURVE ( 'NONE', #6916, #11814, #17610, .T. ) ;
#3677 = CARTESIAN_POINT ( 'NONE',  ( -126.1404785418517918, -15.29729532696464567, -2.500000000000000000 ) ) ;
#3678 = CARTESIAN_POINT ( 'NONE',  ( -10.45209268736360997, -79.61314805016640150, -12.99038105676658539 ) ) ;
#3679 = VERTEX_POINT ( 'NONE', #8863 ) ;
#3680 = CARTESIAN_POINT ( 'NONE',  ( -85.86167379012967160, 34.32252072304513746, 35.00000000000000000 ) ) ;
#3681 = FACE_BOUND ( 'NONE', #6284, .T. ) ;
#3682 = CIRCLE ( 'NONE', #3367, 1.500000000000001332 ) ;
#3683 = DIRECTION ( 'NONE',  ( -0.1566598588826321192, 0.9876526153536342445, 7.798540720466730171E-17 ) ) ;
#3684 = CARTESIAN_POINT ( 'NONE',  ( -20.16390053013728334, -18.38564226699385529, 4.330127018922218518 ) ) ;
#3685 = DIRECTION ( 'NONE',  ( -0.1566598588826321192, 0.9876526153536342445, 7.798540720466730171E-17 ) ) ;
#3686 =( GEOMETRIC_REPRESENTATION_CONTEXT ( 3 ) GLOBAL_UNCERTAINTY_ASSIGNED_CONTEXT ( ( #1542 ) ) GLOBAL_UNIT_ASSIGNED_CONTEXT ( ( #7891, #10795, #3225 ) ) REPRESENTATION_CONTEXT ( 'NONE', 'WORKASPACE' ) );
#3687 = ORIENTED_EDGE ( 'NONE', *, *, #4439, .F. ) ;
#3688 = EDGE_LOOP ( 'NONE', ( #2858, #18740 ) ) ;
#3689 = ORIENTED_EDGE ( 'NONE', *, *, #1480, .F. ) ;
#3690 = PLANE ( 'NONE',  #13481 ) ;
#3691 = FACE_BOUND ( 'NONE', #9396, .T. ) ;
#3692 = EDGE_CURVE ( 'NONE', #11647, #1436, #5046, .T. ) ;
#3693 = EDGE_CURVE ( 'NONE', #3520, #9109, #17414, .T. ) ;
#3694 = EDGE_CURVE ( 'NONE', #344, #7608, #18113, .T. ) ;
#3695 = ORIENTED_EDGE ( 'NONE', *, *, #7288, .F. ) ;
#3696 = EDGE_CURVE ( 'NONE', #16742, #11890, #1730, .T. ) ;
#3697 = AXIS2_PLACEMENT_3D ( 'NONE', #8454, #13163, #2931 ) ;
#3698 = VERTEX_POINT ( 'NONE', #6213 ) ;
#3699 = CARTESIAN_POINT ( 'NONE',  ( -80.30645961545690170, -27.92535762103354458, 92.77853496600735639 ) ) ;
#3700 = FACE_BOUND ( 'NONE', #425, .T. ) ;
#3701 = CARTESIAN_POINT ( 'NONE',  ( 59.44021041145192896, -44.12097743988037735, -20.00000000000000355 ) ) ;
#3702 = DIRECTION ( 'NONE',  ( 1.000000000000000000, 0.000000000000000000, 0.000000000000000000 ) ) ;
#3703 = DIRECTION ( 'NONE',  ( -0.1566598588826321192, 0.9876526153536342445, 7.798540720466730171E-17 ) ) ;
#3704 = CARTESIAN_POINT ( 'NONE',  ( -60.36818477289977380, -29.82528948739119556, 21.65063509461101887 ) ) ;
#3705 = VERTEX_POINT ( 'NONE', #9314 ) ;
#3706 = ORIENTED_EDGE ( 'NONE', *, *, #1080, .T. ) ;
#3707 = DIRECTION ( 'NONE',  ( 3.816390434826605238E-17, 0.000000000000000000, -1.000000000000000000 ) ) ;
#3708 = EDGE_LOOP ( 'NONE', ( #2297, #18656 ) ) ;
#3709 = CYLINDRICAL_SURFACE ( 'NONE', #16272, 1.500000000000001554 ) ;
#3710 = ORIENTED_EDGE ( 'NONE', *, *, #16731, .T. ) ;
#3711 = EDGE_LOOP ( 'NONE', ( #9095, #9230 ) ) ;
#3712 = ORIENTED_EDGE ( 'NONE', *, *, #4114, .T. ) ;
#3713 = CARTESIAN_POINT ( 'NONE',  ( -309.1404785418517918, -2.850701963179328668, 9.951701414186818625E-16 ) ) ;
#3714 = CIRCLE ( 'NONE', #6170, 139.0000000000000000 ) ;
#3715 = CARTESIAN_POINT ( 'NONE',  ( -47.03487446562577645, -27.71038139247565368, 21.65063509461101887 ) ) ;
#3716 = EDGE_CURVE ( 'NONE', #11172, #12170, #17981, .T. ) ;
#3717 = DIRECTION ( 'NONE',  ( -0.9876526153536336894, -0.1566598588826349503, 0.000000000000000000 ) ) ;
#3718 = DIRECTION ( 'NONE',  ( -0.9876526153536341335, -0.1566598588826327021, 0.000000000000000000 ) ) ;
#3719 = EDGE_CURVE ( 'NONE', #1188, #8364, #15093, .T. ) ;
#3720 = VECTOR ( 'NONE', #13608, 1000.000000000000000 ) ;
#3721 = DIRECTION ( 'NONE',  ( -0.9876526153536336894, -0.1566598588826350336, 0.000000000000000000 ) ) ;
#3722 = CARTESIAN_POINT ( 'NONE',  ( -16.70711637639958269, -17.83733276090463704, 21.65063509461101532 ) ) ;
#3723 = CARTESIAN_POINT ( 'NONE',  ( -23.33121169713865584, -23.95054477929251036, 8.660254037844417496 ) ) ;
#3724 = FACE_OUTER_BOUND ( 'NONE', #11173, .T. ) ;
#3725 = ORIENTED_EDGE ( 'NONE', *, *, #6440, .F. ) ;
#3726 = EDGE_LOOP ( 'NONE', ( #17084, #17441, #17181, #12468 ) ) ;
#3727 = LINE ( 'NONE', #9896, #11483 ) ;
#3728 = CARTESIAN_POINT ( 'NONE',  ( -58.68235252892885256, -24.49537676341649117, 17.32050807568882078 ) ) ;
#3729 = ORIENTED_EDGE ( 'NONE', *, *, #10659, .F. ) ;
#3730 = CARTESIAN_POINT ( 'NONE',  ( -47.81817376003892406, -22.77211831570754086, 12.99038105676661736 ) ) ;
#3731 = VERTEX_POINT ( 'NONE', #18067 ) ;
#3732 = EDGE_LOOP ( 'NONE', ( #18641, #6323 ) ) ;
#3733 = CARTESIAN_POINT ( 'NONE',  ( -59.83472345504510770, -87.44614099429799126, 4.330127018922213189 ) ) ;
#3734 = FACE_OUTER_BOUND ( 'NONE', #871, .T. ) ;
#3735 = CARTESIAN_POINT ( 'NONE',  ( 1.360103686702108128, -20.03404830722672259, -17.32050807568878170 ) ) ;
#3736 = DIRECTION ( 'NONE',  ( 0.000000000000000000, 0.000000000000000000, 1.000000000000000000 ) ) ;
#3737 = CARTESIAN_POINT ( 'NONE',  ( -50.45202360918564466, -85.95787233491300583, -17.32050807568878525 ) ) ;
#3738 = DIRECTION ( 'NONE',  ( -0.1566598588826321192, 0.9876526153536342445, 7.798540720466730171E-17 ) ) ;
#3739 =( NAMED_UNIT ( * ) PLANE_ANGLE_UNIT ( ) SI_UNIT ( $, .RADIAN. ) );
#3740 = ADVANCED_FACE ( 'NONE', ( #14914 ), #3428, .F. ) ;
#3741 = DIRECTION ( 'NONE',  ( 1.000000000000000000, 0.000000000000000000, 0.000000000000000000 ) ) ;
#3742 = EDGE_LOOP ( 'NONE', ( #2805, #17397 ) ) ;
#3743 = DIRECTION ( 'NONE',  ( -0.1566598588826321192, 0.9876526153536342445, 7.798540720466730171E-17 ) ) ;
#3744 = DIRECTION ( 'NONE',  ( 0.000000000000000000, 0.000000000000000000, 1.000000000000000000 ) ) ;
#3745 = CYLINDRICAL_SURFACE ( 'NONE', #10609, 1.500000000000000666 ) ;
#3746 = ADVANCED_FACE ( 'NONE', ( #1935 ), #7720, .F. ) ;
#3747 = DIRECTION ( 'NONE',  ( -0.1566598588826321192, 0.9876526153536342445, 7.798540720466730171E-17 ) ) ;
#3748 = VERTEX_POINT ( 'NONE', #6311 ) ;
#3749 = ORIENTED_EDGE ( 'NONE', *, *, #12586, .F. ) ;
#3750 = DIRECTION ( 'NONE',  ( -0.9876526153536336894, -0.1566598588826349503, 0.000000000000000000 ) ) ;
#3751 = CARTESIAN_POINT ( 'NONE',  ( 0.000000000000000000, 0.000000000000000000, 32.00000000000000000 ) ) ;
#3752 = ORIENTED_EDGE ( 'NONE', *, *, #15016, .T. ) ;
#3753 = EDGE_LOOP ( 'NONE', ( #2627, #3140, #11646, #8492 ) ) ;
#3754 = CARTESIAN_POINT ( 'NONE',  ( 55.85952145814821534, 6.938893903907228378E-15, -24.99999999999999289 ) ) ;
#3755 = ORIENTED_EDGE ( 'NONE', *, *, #4446, .T. ) ;
#3756 = CARTESIAN_POINT ( 'NONE',  ( -26.58364252993588650, -19.40393134973095357, -4.330127018922180326 ) ) ;
#3757 = ORIENTED_EDGE ( 'NONE', *, *, #4389, .F. ) ;
#3758 = CARTESIAN_POINT ( 'NONE',  ( -2.200000000000000178, 0.000000000000000000, -25.00000000000000000 ) ) ;
#3759 = LINE ( 'NONE', #12576, #17335 ) ;
#3760 = DIRECTION ( 'NONE',  ( 0.000000000000000000, 0.000000000000000000, 1.000000000000000000 ) ) ;
#3761 = DIRECTION ( 'NONE',  ( -0.1566598588826326743, -0.9876526153536341335, 0.000000000000000000 ) ) ;
#3762 = AXIS2_PLACEMENT_3D ( 'NONE', #5266, #13869, #14273 ) ;
#3763 = ORIENTED_EDGE ( 'NONE', *, *, #2432, .F. ) ;
#3764 = CARTESIAN_POINT ( 'NONE',  ( -2.057045456857756971, -78.28153924966404986, 21.65063509461100821 ) ) ;
#3765 = DIRECTION ( 'NONE',  ( -0.1566598588826321192, 0.9876526153536342445, 7.798540720466730171E-17 ) ) ;
#3766 = EDGE_LOOP ( 'NONE', ( #8570, #391 ) ) ;
#3767 = FACE_BOUND ( 'NONE', #10947, .T. ) ;
#3768 = CARTESIAN_POINT ( 'NONE',  ( -5.842937607509656850, -16.11407431319567962, 17.32050807568881012 ) ) ;
#3769 = DIRECTION ( 'NONE',  ( -0.8007491221077704946, 0.5989998693185457634, 1.888919472620034684E-16 ) ) ;
#3770 = EDGE_CURVE ( 'NONE', #7505, #139, #10809, .T. ) ;
#3771 = CARTESIAN_POINT ( 'NONE',  ( -126.1404785418517918, -2.850701963179328668, -5.500000000000000000 ) ) ;
#3772 = ORIENTED_EDGE ( 'NONE', *, *, #3847, .T. ) ;
#3773 = ORIENTED_EDGE ( 'NONE', *, *, #13251, .T. ) ;
#3774 = EDGE_CURVE ( 'NONE', #12140, #610, #7877, .T. ) ;
#3775 = VERTEX_POINT ( 'NONE', #14690 ) ;
#3776 = ORIENTED_EDGE ( 'NONE', *, *, #11014, .F. ) ;
#3777 = DIRECTION ( 'NONE',  ( -0.9876526153536336894, -0.1566598588826349503, 0.000000000000000000 ) ) ;
#3778 = FACE_BOUND ( 'NONE', #15963, .T. ) ;
#3779 = CARTESIAN_POINT ( 'NONE',  ( -65.26681283949008616, -88.30777021815246997, -17.32050807568878525 ) ) ;
#3780 = AXIS2_PLACEMENT_3D ( 'NONE', #16211, #3203, #13526 ) ;
#3781 = DIRECTION ( 'NONE',  ( -0.9876526153536336894, -0.1566598588826349503, 0.000000000000000000 ) ) ;
#3782 = DIRECTION ( 'NONE',  ( -8.693966348389027220E-17, 1.991237296706375196E-16, -1.000000000000000000 ) ) ;
#3783 = ORIENTED_EDGE ( 'NONE', *, *, #1166, .T. ) ;
#3784 = AXIS2_PLACEMENT_3D ( 'NONE', #17823, #14857, #657 ) ;
#3785 = CARTESIAN_POINT ( 'NONE',  ( -69.25705831108246002, -31.23522821733487476, -17.32050807568878170 ) ) ;
#3786 = DIRECTION ( 'NONE',  ( -0.9876526153536341335, -0.1566598588826327021, 0.000000000000000000 ) ) ;
#3787 = EDGE_CURVE ( 'NONE', #4836, #16919, #17591, .T. ) ;
#3788 = EDGE_LOOP ( 'NONE', ( #12762, #5999, #4570, #11309 ) ) ;
#3789 = DIRECTION ( 'NONE',  ( -0.9876526153536336894, -0.1566598588826349503, 0.000000000000000000 ) ) ;
#3790 = ADVANCED_FACE ( 'NONE', ( #11555 ), #3207, .F. ) ;
#3791 = CARTESIAN_POINT ( 'NONE',  ( -38.92930022185625205, -21.36217958576384746, -8.660254037844380193 ) ) ;
#3792 = EDGE_CURVE ( 'NONE', #18229, #1028, #7333, .T. ) ;
#3793 = DIRECTION ( 'NONE',  ( -0.1566598588826321192, 0.9876526153536342445, 7.798540720466730171E-17 ) ) ;
#3794 = VERTEX_POINT ( 'NONE', #2179 ) ;
#3795 = VERTEX_POINT ( 'NONE', #18247 ) ;
#3796 = FACE_OUTER_BOUND ( 'NONE', #15562, .T. ) ;
#3797 = ORIENTED_EDGE ( 'NONE', *, *, #8887, .F. ) ;
#3798 = CARTESIAN_POINT ( 'NONE',  ( -38.92930022185625205, -21.36217958576385456, 8.660254037844417496 ) ) ;
#3799 = CIRCLE ( 'NONE', #14422, 145.0000000000000284 ) ;
#3800 = FACE_BOUND ( 'NONE', #12522, .T. ) ;
#3801 = CARTESIAN_POINT ( 'NONE',  ( -19.34096622554629263, -81.02308678011010556, 17.32050807568881368 ) ) ;
#3802 = LINE ( 'NONE', #18377, #7555 ) ;
#3803 = DIRECTION ( 'NONE',  ( 0.7999937637212573005, -0.6000083149482994260, 3.937913489109425158E-17 ) ) ;
#3804 = AXIS2_PLACEMENT_3D ( 'NONE', #14685, #1704, #13247 ) ;
#3805 = CARTESIAN_POINT ( 'NONE',  ( -47.98289207080156871, -85.56622268770642847, -4.330127018922185655 ) ) ;
#3806 = LINE ( 'NONE', #12455, #3815 ) ;
#3807 = ORIENTED_EDGE ( 'NONE', *, *, #2766, .F. ) ;
#3808 = CARTESIAN_POINT ( 'NONE',  ( -23.33121169713865584, -23.95054477929251036, -8.660254037844380193 ) ) ;
#3809 = PLANE ( 'NONE',  #9232 ) ;
#3810 = ADVANCED_FACE ( 'NONE', ( #5219 ), #1901, .F. ) ;
#3811 = EDGE_LOOP ( 'NONE', ( #6923, #2569, #17630, #1572 ) ) ;
#3812 = EDGE_LOOP ( 'NONE', ( #14328, #12878 ) ) ;
#3813 = FACE_OUTER_BOUND ( 'NONE', #1325, .T. ) ;
#3814 = CARTESIAN_POINT ( 'NONE',  ( -28.26947477390680774, -24.73384407370567217, -17.32050807568878170 ) ) ;
#3815 = VECTOR ( 'NONE', #12623, 1000.000000000000000 ) ;
#3816 = ORIENTED_EDGE ( 'NONE', *, *, #4057, .F. ) ;
#3817 = CIRCLE ( 'NONE', #16884, 1.499999999999999556 ) ;
#3818 = EDGE_CURVE ( 'NONE', #13180, #3665, #10582, .T. ) ;
#3819 = CIRCLE ( 'NONE', #18435, 1.500000000000000888 ) ;
#3820 = ORIENTED_EDGE ( 'NONE', *, *, #3504, .T. ) ;
#3821 = DIRECTION ( 'NONE',  ( -0.1566598588826321192, 0.9876526153536342445, 7.798540720466730171E-17 ) ) ;
#3822 = EDGE_CURVE ( 'NONE', #9967, #1267, #5463, .T. ) ;
#3823 = CIRCLE ( 'NONE', #13813, 1.500000000000000888 ) ;
#3824 = DIRECTION ( 'NONE',  ( -0.1566598588826321747, 0.9876526153536343555, 0.000000000000000000 ) ) ;
#3825 = DIRECTION ( 'NONE',  ( -0.1566598588826321747, 0.9876526153536343555, 0.000000000000000000 ) ) ;
#3826 = ORIENTED_EDGE ( 'NONE', *, *, #15472, .T. ) ;
#3827 = DIRECTION ( 'NONE',  ( 0.000000000000000000, 0.000000000000000000, 1.000000000000000000 ) ) ;
#3828 = DIRECTION ( 'NONE',  ( -0.1566598588826321747, 0.9876526153536343555, 0.000000000000000000 ) ) ;
#3829 = AXIS2_PLACEMENT_3D ( 'NONE', #12912, #5839, #4306 ) ;
#3830 = STYLED_ITEM ( 'NONE', ( #1104 ), #1445 ) ;
#3831 = CARTESIAN_POINT ( 'NONE',  ( -49.79347899074618056, -23.08543803347280132, -4.330127018922180326 ) ) ;
#3832 = PRESENTATION_STYLE_ASSIGNMENT (( #16865 ) ) ;
#3833 = CARTESIAN_POINT ( 'NONE',  ( -89.14047854185180597, 6.938893903907228378E-15, -30.00000000000000000 ) ) ;
#3834 = ORIENTED_EDGE ( 'NONE', *, *, #8638, .F. ) ;
#3835 = CARTESIAN_POINT ( 'NONE',  ( -22.34355908178503114, -23.79388492040988012, -12.99038105676658006 ) ) ;
#3836 = AXIS2_PLACEMENT_3D ( 'NONE', #17698, #13386, #12037 ) ;
#3837 = CARTESIAN_POINT ( 'NONE',  ( -27.73601345605213098, -82.35469558061247142, -8.660254037844385522 ) ) ;
#3838 = VERTEX_POINT ( 'NONE', #9282 ) ;
#3839 = CARTESIAN_POINT ( 'NONE',  ( -83.69844302882627574, 31.44749966561626664, 35.00001199999999812 ) ) ;
#3840 = CARTESIAN_POINT ( 'NONE',  ( -73.49714175923330117, -26.84527464665595176, -17.32050807568878170 ) ) ;
#3842 = ORIENTED_EDGE ( 'NONE', *, *, #1417, .F. ) ;
#3841 = LINE ( 'NONE', #9655, #2706 ) ;
#3843 = CARTESIAN_POINT ( 'NONE',  ( -170.3665179301995352, 31.30647307655612366, 9.951701414186830458E-16 ) ) ;
#3844 = ORIENTED_EDGE ( 'NONE', *, *, #6220, .F. ) ;
#3845 = PRODUCT_DEFINITION_FORMATION_WITH_SPECIFIED_SOURCE ( 'ANY', '', #775, .NOT_KNOWN. ) ;
#3846 = EDGE_LOOP ( 'NONE', ( #11783, #18763 ) ) ;
#3847 = EDGE_CURVE ( 'NONE', #7962, #9877, #480, .T. ) ;
#3848 = VECTOR ( 'NONE', #9283, 1000.000000000000000 ) ;
#3849 = VERTEX_POINT ( 'NONE', #14879 ) ;
#3850 = EDGE_CURVE ( 'NONE', #12551, #2681, #2721, .T. ) ;
#3851 = LINE ( 'NONE', #15156, #12443 ) ;
#3852 = EDGE_CURVE ( 'NONE', #12162, #1839, #928, .T. ) ;
#3853 = CIRCLE ( 'NONE', #5998, 1.500000000000000888 ) ;
#3854 = DIRECTION ( 'NONE',  ( -0.1566598588826321192, 0.9876526153536342445, 7.798540720466731404E-17 ) ) ;
#3855 = DIRECTION ( 'NONE',  ( -0.1566598588826321192, 0.9876526153536342445, 7.798540720466731404E-17 ) ) ;
#3856 = DIRECTION ( 'NONE',  ( -0.1566598588826321192, 0.9876526153536342445, 7.798540720466730171E-17 ) ) ;
#3857 = CIRCLE ( 'NONE', #8432, 1.500000000000000888 ) ;
#3858 = CYLINDRICAL_SURFACE ( 'NONE', #16978, 1.500000000000000666 ) ;
#3859 = CARTESIAN_POINT ( 'NONE',  ( -19.34096622554629263, -81.02308678011010556, 8.660254037844412167 ) ) ;
#3860 = CARTESIAN_POINT ( 'NONE',  ( -5.513829610595458064, -78.82984875575324679, -21.65063509461098690 ) ) ;
#3861 = COLOUR_RGB ( '', 0.08235294, 0.09019608, 0.10196078) ;
#3862 = CARTESIAN_POINT ( 'NONE',  ( -6.995308533625909320, -79.06483854407720457, -12.99038105676658539 ) ) ;
#3863 = DIRECTION ( 'NONE',  ( -0.1566598588826321747, 0.9876526153536343555, 0.000000000000000000 ) ) ;
#3864 = VERTEX_POINT ( 'NONE', #3393 ) ;
#3865 = CARTESIAN_POINT ( 'NONE',  ( -28.26947477390680774, -24.73384407370567217, 1.869203119972154228E-14 ) ) ;
#3866 = EDGE_LOOP ( 'NONE', ( #8102, #11142 ) ) ;
#3867 = LINE ( 'NONE', #8060, #10761 ) ;
#3868 = CIRCLE ( 'NONE', #14792, 155.0000000000000284 ) ;
#3869 = AXIS2_PLACEMENT_3D ( 'NONE', #6572, #9503, #16820 ) ;
#3870 = FACE_BOUND ( 'NONE', #1085, .T. ) ;
#3871 = ADVANCED_FACE ( 'NONE', ( #582 ), #15062, .F. ) ;
#3872 =( LENGTH_UNIT ( ) NAMED_UNIT ( * ) SI_UNIT ( .MILLI., .METRE. ) );
#3873 = AXIS2_PLACEMENT_3D ( 'NONE', #8173, #994, #6765 ) ;
#3874 = CIRCLE ( 'NONE', #16614, 2.000000000000000000 ) ;
#3875 = CARTESIAN_POINT ( 'NONE',  ( -25.76070822534488869, -82.04137586284721806, 8.660254037844412167 ) ) ;
#3876 = EDGE_CURVE ( 'NONE', #12785, #12633, #6616, .T. ) ;
#3877 = AXIS2_PLACEMENT_3D ( 'NONE', #11321, #11240, #9546 ) ;
#3878 = DIRECTION ( 'NONE',  ( 1.000000000000000000, 0.000000000000000000, 0.000000000000000000 ) ) ;
#3879 = DIRECTION ( 'NONE',  ( -0.000000000000000000, -0.000000000000000000, -1.000000000000000000 ) ) ;
#3880 = VECTOR ( 'NONE', #18023, 1000.000000000000000 ) ;
#3881 = EDGE_CURVE ( 'NONE', #10603, #16711, #2422, .T. ) ;
#3882 = DIRECTION ( 'NONE',  ( -0.1566598588826321192, 0.9876526153536342445, 7.798540720466731404E-17 ) ) ;
#3883 = LINE ( 'NONE', #17104, #1489 ) ;
#3884 = DIRECTION ( 'NONE',  ( 0.000000000000000000, 0.000000000000000000, 1.000000000000000000 ) ) ;
#3885 = ORIENTED_EDGE ( 'NONE', *, *, #2261, .T. ) ;
#3886 = DIRECTION ( 'NONE',  ( -0.9876526153536341335, -0.1566598588826327021, 0.000000000000000000 ) ) ;
#3887 = DIRECTION ( 'NONE',  ( -1.000000000000000000, 0.000000000000000000, 0.000000000000000000 ) ) ;
#3888 = ORIENTED_EDGE ( 'NONE', *, *, #1904, .F. ) ;
#3889 = ORIENTED_EDGE ( 'NONE', *, *, #6388, .T. ) ;
#3890 = DIRECTION ( 'NONE',  ( -0.1566598588826321192, 0.9876526153536342445, 7.798540720466730171E-17 ) ) ;
#3891 = CARTESIAN_POINT ( 'NONE',  ( -128.4401431403265121, -15.07824538754614352, 3.563338245596200160 ) ) ;
#3892 = CARTESIAN_POINT ( 'NONE',  ( -170.3886569253285188, 32.16932146890094657, 4.579216830445319353 ) ) ;
#3893 = CIRCLE ( 'NONE', #18199, 12.74754878398196567 ) ;
#3894 = VERTEX_POINT ( 'NONE', #2440 ) ;
#3895 = EDGE_CURVE ( 'NONE', #16215, #2189, #939, .T. ) ;
#3896 = CIRCLE ( 'NONE', #12685, 1.500000000000000000 ) ;
#3897 = AXIS2_PLACEMENT_3D ( 'NONE', #5898, #17199, #14618 ) ;
#3898 = FACE_OUTER_BOUND ( 'NONE', #9715, .T. ) ;
#3899 = EDGE_CURVE ( 'NONE', #1264, #10247, #15441, .T. ) ;
#3900 = CARTESIAN_POINT ( 'NONE',  ( -73.43026588874043625, 46.45959363168854139, 2.666351014094141547 ) ) ;
#3901 = DIRECTION ( 'NONE',  ( 1.000000000000000000, 0.000000000000000000, 0.000000000000000000 ) ) ;
#3902 = EDGE_CURVE ( 'NONE', #7759, #139, #10286, .T. ) ;
#3903 = DIRECTION ( 'NONE',  ( -0.1566598588826321192, 0.9876526153536342445, 7.798540720466731404E-17 ) ) ;
#3904 = VECTOR ( 'NONE', #856, 1000.000000000000000 ) ;
#3905 = CYLINDRICAL_SURFACE ( 'NONE', #10272, 1.500000000000000888 ) ;
#3907 = DIRECTION ( 'NONE',  ( 0.000000000000000000, 0.000000000000000000, 1.000000000000000000 ) ) ;
#3906 = CIRCLE ( 'NONE', #6372, 1.500000000000000888 ) ;
#3908 = VERTEX_POINT ( 'NONE', #15801 ) ;
#3909 = DIRECTION ( 'NONE',  ( -0.1566598588826321747, 0.9876526153536343555, 0.000000000000000000 ) ) ;
#3910 = DIRECTION ( 'NONE',  ( -0.1566598588826321192, 0.9876526153536342445, 7.798540720466730171E-17 ) ) ;
#3911 = AXIS2_PLACEMENT_3D ( 'NONE', #16364, #12158, #3354 ) ;
#3912 = ORIENTED_EDGE ( 'NONE', *, *, #10157, .F. ) ;
#3913 = ORIENTED_EDGE ( 'NONE', *, *, #1417, .T. ) ;
#3914 = FACE_BOUND ( 'NONE', #14625, .T. ) ;
#3915 = CARTESIAN_POINT ( 'NONE',  ( -2.096680467035594297, -20.58235781331593017, -17.32050807568878170 ) ) ;
#3916 = ORIENTED_EDGE ( 'NONE', *, *, #8270, .F. ) ;
#3917 = VERTEX_POINT ( 'NONE', #12927 ) ;
#3918 = DIRECTION ( 'NONE',  ( -0.1566598588826321747, 0.9876526153536343555, 0.000000000000000000 ) ) ;
#3919 = ORIENTED_EDGE ( 'NONE', *, *, #12136, .T. ) ;
#3920 = ORIENTED_EDGE ( 'NONE', *, *, #12842, .T. ) ;
#3921 = DIRECTION ( 'NONE',  ( 0.000000000000000000, 0.000000000000000000, 1.000000000000000000 ) ) ;
#3922 = AXIS2_PLACEMENT_3D ( 'NONE', #7381, #10297, #13135 ) ;
#3923 = EDGE_CURVE ( 'NONE', #14148, #17176, #6071, .T. ) ;
#3924 = CIRCLE ( 'NONE', #11192, 1.500000000000000888 ) ;
#3925 = DIRECTION ( 'NONE',  ( 0.000000000000000000, 0.000000000000000000, 1.000000000000000000 ) ) ;
#3926 = EDGE_CURVE ( 'NONE', #10692, #9818, #15739, .T. ) ;
#3927 = VERTEX_POINT ( 'NONE', #3931 ) ;
#3928 = AXIS2_PLACEMENT_3D ( 'NONE', #18459, #13840, #16618 ) ;
#3929 = EDGE_CURVE ( 'NONE', #7929, #6801, #5095, .T. ) ;
#3930 = DIRECTION ( 'NONE',  ( -0.9201637183752248150, 0.3915338189555022108, 0.000000000000000000 ) ) ;
#3931 = CARTESIAN_POINT ( 'NONE',  ( -70.04035760549561473, -26.29696514056674772, 1.908195823574487804E-14 ) ) ;
#3932 = ADVANCED_FACE ( 'NONE', ( #14665 ), #3173, .F. ) ;
#3933 = CARTESIAN_POINT ( 'NONE',  ( -136.4286012789710867, -132.1908753210555574, 5.500000000000000000 ) ) ;
#3934 = CIRCLE ( 'NONE', #16992, 1.500000000000000444 ) ;
#3935 = DIRECTION ( 'NONE',  ( -0.1566598588826321192, 0.9876526153536342445, 7.798540720466730171E-17 ) ) ;
#3936 = PRODUCT ( 'Ergonomic Handle Grip Sleeves', 'Ergonomic Handle Grip Sleeves', '', ( #17404 ) ) ;
#3937 = FACE_OUTER_BOUND ( 'NONE', #2169, .T. ) ;
#3938 = ORIENTED_EDGE ( 'NONE', *, *, #1214, .T. ) ;
#3939 = CARTESIAN_POINT ( 'NONE',  ( -65.26681283949008616, -88.30777021815248418, 17.32050807568881368 ) ) ;
#3940 = AXIS2_PLACEMENT_3D ( 'NONE', #11869, #5850, #7643 ) ;
#3941 = CYLINDRICAL_SURFACE ( 'NONE', #7791, 1.500000000000001554 ) ;
#3942 = CARTESIAN_POINT ( 'NONE',  ( -11.93357161039406300, -79.84813783849037350, 4.330127018922213189 ) ) ;
#3943 = CARTESIAN_POINT ( 'NONE',  ( -34.97868976044173195, -20.73554015023332298, -12.99038105676658006 ) ) ;
#3944 = ORIENTED_EDGE ( 'NONE', *, *, #1956, .F. ) ;
#3945 = CARTESIAN_POINT ( 'NONE',  ( -21.81009776393036503, -81.41473642731669713, 21.65063509461101532 ) ) ;
#3946 = FACE_OUTER_BOUND ( 'NONE', #12937, .T. ) ;
#3947 = ORIENTED_EDGE ( 'NONE', *, *, #12727, .F. ) ;
#3948 = AXIS2_PLACEMENT_3D ( 'NONE', #18597, #15587, #9741 ) ;
#3949 = DIRECTION ( 'NONE',  ( 0.000000000000000000, 0.000000000000000000, 1.000000000000000000 ) ) ;
#3950 = DIRECTION ( 'NONE',  ( -0.9876526153536336894, -0.1566598588826349503, 0.000000000000000000 ) ) ;
#3951 = ADVANCED_FACE ( 'NONE', ( #6149 ), #831, .F. ) ;
#3952 = ORIENTED_EDGE ( 'NONE', *, *, #10858, .T. ) ;
#3953 = AXIS2_PLACEMENT_3D ( 'NONE', #14667, #17923, #6341 ) ;
#3954 = LINE ( 'NONE', #9767, #17994 ) ;
#3955 = DIRECTION ( 'NONE',  ( -0.9876526153536341335, -0.1566598588826327021, 0.000000000000000000 ) ) ;
#3956 = CARTESIAN_POINT ( 'NONE',  ( -76.90911978745816668, 1.387778780781445676E-14, -25.00000000000000000 ) ) ;
#3957 = DIRECTION ( 'NONE',  ( -0.9876526153536336894, -0.1566598588826350336, 0.000000000000000000 ) ) ;
#3958 = AXIS2_PLACEMENT_3D ( 'NONE', #6974, #13097, #15766 ) ;
#3959 = CARTESIAN_POINT ( 'NONE',  ( 73.09088021254186174, 1.387778780781445676E-14, -19.99999999999999645 ) ) ;
#3960 = EDGE_LOOP ( 'NONE', ( #2107, #7180 ) ) ;
#3961 = FACE_OUTER_BOUND ( 'NONE', #10938, .T. ) ;
#3962 = EDGE_CURVE ( 'NONE', #5781, #10329, #4541, .T. ) ;
#3963 = AXIS2_PLACEMENT_3D ( 'NONE', #14828, #522, #11945 ) ;
#3964 = ADVANCED_FACE ( 'NONE', ( #8143 ), #5303, .F. ) ;
#3965 = FACE_OUTER_BOUND ( 'NONE', #11098, .T. ) ;
#3966 = CARTESIAN_POINT ( 'NONE',  ( 11.59211860341528144, 6.314490184041265053, -130.3485206753969976 ) ) ;
#3967 = AXIS2_PLACEMENT_3D ( 'NONE', #1146, #9926, #1335 ) ;
#3968 = AXIS2_PLACEMENT_3D ( 'NONE', #3418, #2106, #7894 ) ;
#3969 = ORIENTED_EDGE ( 'NONE', *, *, #5996, .F. ) ;
#3970 = CARTESIAN_POINT ( 'NONE',  ( -48.02252708097939404, -27.86704125135830523, 8.660254037844417496 ) ) ;
#3971 = VERTEX_POINT ( 'NONE', #12287 ) ;
#3972 = ORIENTED_EDGE ( 'NONE', *, *, #16312, .F. ) ;
#3973 = DIRECTION ( 'NONE',  ( 1.000000000000000000, 0.000000000000000000, 0.000000000000000000 ) ) ;
#3974 = CIRCLE ( 'NONE', #13966, 1.499999999999999556 ) ;
#3975 = VERTEX_POINT ( 'NONE', #1245 ) ;
#3976 = ORIENTED_EDGE ( 'NONE', *, *, #14274, .T. ) ;
#3977 = FACE_BOUND ( 'NONE', #18521, .T. ) ;
#3978 = DIRECTION ( 'NONE',  ( -0.1566598588826321192, 0.9876526153536342445, 7.798540720466730171E-17 ) ) ;
#3979 = CIRCLE ( 'NONE', #10651, 1.500000000000000888 ) ;
#3980 = CARTESIAN_POINT ( 'NONE',  ( -25.10216360690543524, -19.16894156140701000, -4.330127018922180326 ) ) ;
#3981 = EDGE_CURVE ( 'NONE', #1864, #9740, #5131, .T. ) ;
#3982 = AXIS2_PLACEMENT_3D ( 'NONE', #7370, #7185, #6027 ) ;
#3983 = CARTESIAN_POINT ( 'NONE',  ( -66.08974714408108753, -25.67032570503621258, -21.65063509461097979 ) ) ;
#3984 = DIRECTION ( 'NONE',  ( -0.1566598588826321192, 0.9876526153536342445, 7.798540720466730171E-17 ) ) ;
#3985 = DIRECTION ( 'NONE',  ( -0.9876526153536341335, -0.1566598588826327021, 0.000000000000000000 ) ) ;
#3986 = ORIENTED_EDGE ( 'NONE', *, *, #6473, .F. ) ;
#3987 = DIRECTION ( 'NONE',  ( 0.000000000000000000, 0.000000000000000000, 1.000000000000000000 ) ) ;
#3988 = ADVANCED_FACE ( 'NONE', ( #3946 ), #5492, .F. ) ;
#3989 = VERTEX_POINT ( 'NONE', #10835 ) ;
#3990 = ORIENTED_EDGE ( 'NONE', *, *, #7662, .T. ) ;
#3991 = ORIENTED_EDGE ( 'NONE', *, *, #955, .T. ) ;
#3992 = DIRECTION ( 'NONE',  ( -0.9876526153536341335, -0.1566598588826327021, 0.000000000000000000 ) ) ;
#3993 = ORIENTED_EDGE ( 'NONE', *, *, #6093, .F. ) ;
#3994 = ORIENTED_EDGE ( 'NONE', *, *, #17207, .T. ) ;
#3995 = ORIENTED_EDGE ( 'NONE', *, *, #15798, .F. ) ;
#3996 = ORIENTED_EDGE ( 'NONE', *, *, #9746, .T. ) ;
#3997 = DIRECTION ( 'NONE',  ( -0.000000000000000000, -0.000000000000000000, -1.000000000000000000 ) ) ;
#3998 = EDGE_CURVE ( 'NONE', #18092, #13174, #12065, .T. ) ;
#3999 = DIRECTION ( 'NONE',  ( -0.9876526153536341335, -0.1566598588826327021, 0.000000000000000000 ) ) ;
#4000 = ORIENTED_EDGE ( 'NONE', *, *, #8473, .T. ) ;
#4001 = STYLED_ITEM ( 'NONE', ( #9125 ), #8651 ) ;
#4002 = DIRECTION ( 'NONE',  ( -0.1566598588826321192, 0.9876526153536342445, 7.798540720466730171E-17 ) ) ;
#4003 = CONTEXT_DEPENDENT_SHAPE_REPRESENTATION ( #4342, #9859 ) ;
#4004 = CYLINDRICAL_SURFACE ( 'NONE', #6049, 1.500000000000001554 ) ;
#4005 = CARTESIAN_POINT ( 'NONE',  ( -75.96627329761737712, -27.23692429386254688, 21.65063509461102242 ) ) ;
#4006 = DIRECTION ( 'NONE',  ( -0.1566598588826321192, 0.9876526153536342445, 7.798540720466731404E-17 ) ) ;
#4007 = CARTESIAN_POINT ( 'NONE',  ( -46.54104815794895700, -27.63205146303435100, 1.887572821959364500E-14 ) ) ;
#4008 = ORIENTED_EDGE ( 'NONE', *, *, #145, .T. ) ;
#4009 = ORIENTED_EDGE ( 'NONE', *, *, #484, .F. ) ;
#4010 = CIRCLE ( 'NONE', #10373, 1.500000000000000000 ) ;
#4011 = FACE_BOUND ( 'NONE', #7147, .T. ) ;
#4012 = CARTESIAN_POINT ( 'NONE',  ( -65.26681283949008616, -88.30777021815246997, -8.660254037844385522 ) ) ;
#4013 = EDGE_CURVE ( 'NONE', #9877, #11838, #11025, .T. ) ;
#4014 = ORIENTED_EDGE ( 'NONE', *, *, #7861, .F. ) ;
#4015 = ORIENTED_EDGE ( 'NONE', *, *, #2195, .F. ) ;
#4016 = DIRECTION ( 'NONE',  ( -0.1566598588826321192, 0.9876526153536342445, 7.798540720466730171E-17 ) ) ;
#4017 = ORIENTED_EDGE ( 'NONE', *, *, #13225, .F. ) ;
#4018 = CARTESIAN_POINT ( 'NONE',  ( 8.807133312032172867, -76.55828080195509244, 8.660254037844406838 ) ) ;
#4019 = EDGE_CURVE ( 'NONE', #2560, #14180, #12740, .T. ) ;
#4020 = DIRECTION ( 'NONE',  ( 0.000000000000000000, 0.000000000000000000, 1.000000000000000000 ) ) ;
#4021 = ORIENTED_EDGE ( 'NONE', *, *, #13424, .T. ) ;
#4022 = DIRECTION ( 'NONE',  ( -0.9876526153536341335, -0.1566598588826327021, 0.000000000000000000 ) ) ;
#4023 = VECTOR ( 'NONE', #12780, 1000.000000000000000 ) ;
#4024 = DIRECTION ( 'NONE',  ( -0.000000000000000000, -0.000000000000000000, -1.000000000000000000 ) ) ;
#4025 = LINE ( 'NONE', #9826, #13983 ) ;
#4026 = DIRECTION ( 'NONE',  ( -0.1566598588826321192, 0.9876526153536342445, 7.798540720466730171E-17 ) ) ;
#4027 = VERTEX_POINT ( 'NONE', #15006 ) ;
#4028 = EDGE_CURVE ( 'NONE', #3313, #17816, #1741, .T. ) ;
#4029 = DIRECTION ( 'NONE',  ( 1.000000000000000000, 0.000000000000000000, 0.000000000000000000 ) ) ;
#4030 = CARTESIAN_POINT ( 'NONE',  ( -23.33121169713865584, -23.95054477929251036, 8.660254037844417496 ) ) ;
#4031 = FACE_OUTER_BOUND ( 'NONE', #14769, .T. ) ;
#4032 = ORIENTED_EDGE ( 'NONE', *, *, #6709, .F. ) ;
#4033 = EDGE_LOOP ( 'NONE', ( #13267, #3342 ) ) ;
#4034 = CARTESIAN_POINT ( 'NONE',  ( -79.50650145259169221, 31.87494681980769684, 35.00000599999999906 ) ) ;
#4036 = VERTEX_POINT ( 'NONE', #14821 ) ;
#4035 = FACE_OUTER_BOUND ( 'NONE', #1789, .T. ) ;
#4037 = EDGE_LOOP ( 'NONE', ( #17040, #8717, #14369, #33 ) ) ;
#4038 = ADVANCED_FACE ( 'NONE', ( #11937 ), #3616, .F. ) ;
#4039 = ADVANCED_FACE ( 'NONE', ( #15092 ), #14236, .T. ) ;
#4040 = VERTEX_POINT ( 'NONE', #1934 ) ;
#4041 = VERTEX_POINT ( 'NONE', #5030 ) ;
#4042 = EDGE_CURVE ( 'NONE', #10626, #3227, #8172, .T. ) ;
#4043 = VERTEX_POINT ( 'NONE', #8076 ) ;
#4044 = LINE ( 'NONE', #11339, #8531 ) ;
#4045 = ORIENTED_EDGE ( 'NONE', *, *, #2005, .T. ) ;
#4046 = CARTESIAN_POINT ( 'NONE',  ( -23.12685837619818940, -18.85562184364174598, 4.330127018922218518 ) ) ;
#4047 = CARTESIAN_POINT ( 'NONE',  ( -20.86208015875457988, -23.55889513208593655, -21.65063509461098334 ) ) ;
#4048 = CARTESIAN_POINT ( 'NONE',  ( -346.6053245638183853, 10.98772995598034008, 9.951701414186830458E-16 ) ) ;
#4049 = CYLINDRICAL_SURFACE ( 'NONE', #9045, 1.500000000000001554 ) ;
#4050 = CARTESIAN_POINT ( 'NONE',  ( 3.231158466157551423, 19.73726462726227737, 35.00000000000000000 ) ) ;
#4051 = FACE_BOUND ( 'NONE', #12098, .T. ) ;
#4052 = DIRECTION ( 'NONE',  ( -0.000000000000000000, -0.000000000000000000, 1.000000000000000000 ) ) ;
#4053 = VECTOR ( 'NONE', #14886, 1000.000000000000000 ) ;
#4054 = LINE ( 'NONE', #6840, #16648 ) ;
#4055 = EDGE_LOOP ( 'NONE', ( #6042, #10786 ) ) ;
#4056 = ADVANCED_FACE ( 'NONE', ( #18276 ), #10999, .F. ) ;
#4058 = VERTEX_POINT ( 'NONE', #2388 ) ;
#4057 = EDGE_CURVE ( 'NONE', #14743, #12954, #8778, .T. ) ;
#4059 = CYLINDRICAL_SURFACE ( 'NONE', #9053, 1.500000000000001554 ) ;
#4060 = ORIENTED_EDGE ( 'NONE', *, *, #3528, .T. ) ;
#4061 = ORIENTED_EDGE ( 'NONE', *, *, #16832, .T. ) ;
#4062 = LINE ( 'NONE', #15548, #12899 ) ;
#4063 = EDGE_CURVE ( 'NONE', #6818, #13999, #4246, .T. ) ;
#4064 = EDGE_CURVE ( 'NONE', #14647, #14006, #7892, .T. ) ;
#4065 = FACE_BOUND ( 'NONE', #4543, .T. ) ;
#4066 = ADVANCED_FACE ( 'NONE', ( #16879 ), #5206, .F. ) ;
#4067 =( NAMED_UNIT ( * ) PLANE_ANGLE_UNIT ( ) SI_UNIT ( $, .RADIAN. ) );
#4068 = ORIENTED_EDGE ( 'NONE', *, *, #12819, .T. ) ;
#4069 = DIRECTION ( 'NONE',  ( -0.9876526153536336894, -0.1566598588826349503, 0.000000000000000000 ) ) ;
#4070 = FACE_OUTER_BOUND ( 'NONE', #11082, .T. ) ;
#4071 = EDGE_LOOP ( 'NONE', ( #7725, #18637, #16808, #10084 ) ) ;
#4072 = VERTEX_POINT ( 'NONE', #13625 ) ;
#4073 = ORIENTED_EDGE ( 'NONE', *, *, #9817, .T. ) ;
#4074 = DIRECTION ( 'NONE',  ( -0.1566598588826321192, 0.9876526153536342445, 7.798540720466731404E-17 ) ) ;
#4075 = FACE_OUTER_BOUND ( 'NONE', #11055, .T. ) ;
#4076 = DIRECTION ( 'NONE',  ( -0.000000000000000000, -0.000000000000000000, -1.000000000000000000 ) ) ;
#4077 = AXIS2_PLACEMENT_3D ( 'NONE', #5553, #2600, #8384 ) ;
#4078 = ORIENTED_EDGE ( 'NONE', *, *, #17715, .F. ) ;
#4079 = ORIENTED_EDGE ( 'NONE', *, *, #15226, .F. ) ;
#4080 = EDGE_LOOP ( 'NONE', ( #7014, #5618, #2294, #1360, #5467, #8933, #13419, #8424, #14819, #5962, #5132 ) ) ;
#4081 = DIRECTION ( 'NONE',  ( 0.000000000000000000, 0.000000000000000000, 1.000000000000000000 ) ) ;
#4082 = VERTEX_POINT ( 'NONE', #12281 ) ;
#4083 = ORIENTED_EDGE ( 'NONE', *, *, #11826, .T. ) ;
#4084 = FACE_BOUND ( 'NONE', #5231, .T. ) ;
#4085 = ADVANCED_FACE ( 'NONE', ( #6453 ), #18233, .F. ) ;
#4086 = CARTESIAN_POINT ( 'NONE',  ( -57.69469991357524208, -24.33871690453385028, -4.330127018922180326 ) ) ;
#4087 = EDGE_CURVE ( 'NONE', #4380, #12710, #2739, .T. ) ;
#4088 = PRODUCT_DEFINITION_SHAPE ( 'NONE', 'NONE',  #18801 ) ;
#4089 = CIRCLE ( 'NONE', #12570, 3.000000000000000888 ) ;
#4090 = CARTESIAN_POINT ( 'NONE',  ( -43.04462899403340970, -84.78292339329327376, 4.330127018922213189 ) ) ;
#4091 = PRODUCT_DEFINITION_CONTEXT ( 'detailed design', #8228, 'design' ) ;
#4092 = EDGE_CURVE ( 'NONE', #18200, #6686, #11794, .T. ) ;
#4093 = CIRCLE ( 'NONE', #5625, 1.500000000000000888 ) ;
#4094 = DIRECTION ( 'NONE',  ( -0.9876526153536336894, -0.1566598588826349503, 0.000000000000000000 ) ) ;
#4095 = ITEM_DEFINED_TRANSFORMATION ( 'NONE', 'NONE', #14454,  #18772 ) ;
#4096 = CARTESIAN_POINT ( 'NONE',  ( 0.000000000000000000, 0.000000000000000000, 35.00000000000000000 ) ) ;
#4097 = CARTESIAN_POINT ( 'NONE',  ( -128.1404785157144204, -15.33290121937806205, -2.500000000000000000 ) ) ;
#4098 = ORIENTED_EDGE ( 'NONE', *, *, #3716, .T. ) ;
#4099 = CARTESIAN_POINT ( 'NONE',  ( 7.819480696678551723, -76.71494066083772623, -12.99038105676658894 ) ) ;
#4100 = CARTESIAN_POINT ( 'NONE',  ( -46.33669483700847280, -22.53712852738359729, 21.65063509461102242 ) ) ;
#4101 = VERTEX_POINT ( 'NONE', #7738 ) ;
#4102 = VERTEX_POINT ( 'NONE', #9634 ) ;
#4103 = FACE_BOUND ( 'NONE', #17791, .T. ) ;
#4104 = DIRECTION ( 'NONE',  ( -0.000000000000000000, -0.000000000000000000, -1.000000000000000000 ) ) ;
#4105 = CIRCLE ( 'NONE', #5933, 1.500000000000000444 ) ;
#4106 = DIRECTION ( 'NONE',  ( 0.000000000000000000, 0.000000000000000000, -1.000000000000000000 ) ) ;
#4107 = VECTOR ( 'NONE', #14588, 1000.000000000000000 ) ;
#4108 = EDGE_LOOP ( 'NONE', ( #17122, #7204 ) ) ;
#4109 = FACE_OUTER_BOUND ( 'NONE', #15467, .T. ) ;
#4110 = CARTESIAN_POINT ( 'NONE',  ( -4.361458684479201153, -15.87908452487173427, 1.561251128379126385E-14 ) ) ;
#4111 = ORIENTED_EDGE ( 'NONE', *, *, #15798, .T. ) ;
#4112 = DIRECTION ( 'NONE',  ( -0.9876526153536336894, -0.1566598588826349503, 0.000000000000000000 ) ) ;
#4113 = AXIS2_PLACEMENT_3D ( 'NONE', #14799, #7611, #12017 ) ;
#4114 = EDGE_CURVE ( 'NONE', #5804, #7971, #7933, .T. ) ;
#4115 = CARTESIAN_POINT ( 'NONE',  ( -53.90880776292333820, -86.50618184100221697, 1.424741226644455312E-14 ) ) ;
#4116 = FACE_OUTER_BOUND ( 'NONE', #5413, .T. ) ;
#4117 = LINE ( 'NONE', #5286, #14508 ) ;
#4118 = ORIENTED_EDGE ( 'NONE', *, *, #1350, .F. ) ;
#4119 = DIRECTION ( 'NONE',  ( -0.1566598588826321192, 0.9876526153536342445, 7.798540720466730171E-17 ) ) ;
#4120 = ORIENTED_EDGE ( 'NONE', *, *, #12728, .T. ) ;
#4121 = ADVANCED_FACE ( 'NONE', ( #16952 ), #6603, .F. ) ;
#4122 = CARTESIAN_POINT ( 'NONE',  ( -15.92381708198643153, -22.77559583767277473, 4.330127018922217630 ) ) ;
#4123 = CARTESIAN_POINT ( 'NONE',  ( -38.10636591726525069, -83.99962409888011905, 4.330127018922213189 ) ) ;
#4124 = ORIENTED_EDGE ( 'NONE', *, *, #13537, .T. ) ;
#4125 = ORIENTED_EDGE ( 'NONE', *, *, #16207, .F. ) ;
#4126 = CARTESIAN_POINT ( 'NONE',  ( 2.000000000000000000, 2.449293598294706414E-16, 35.00000000000000000 ) ) ;
#4127 = EDGE_CURVE ( 'NONE', #10862, #9895, #1035, .T. ) ;
#4128 = CARTESIAN_POINT ( 'NONE',  ( -77.95464380949736949, 0.4739080578470992178, 4.432241562448437477 ) ) ;
#4130 = VERTEX_POINT ( 'NONE', #8110 ) ;
#4129 = CARTESIAN_POINT ( 'NONE',  ( -68.55887868246516348, -26.06197535224280770, 17.32050807568882078 ) ) ;
#4131 = AXIS2_PLACEMENT_3D ( 'NONE', #11782, #7456, #15981 ) ;
#4132 = CIRCLE ( 'NONE', #18098, 2.000000000000000000 ) ;
#4133 = CYLINDRICAL_SURFACE ( 'NONE', #15433, 1.500000000000001554 ) ;
#4134 = CARTESIAN_POINT ( 'NONE',  ( -56.91140061916208737, -29.27697998130198442, -12.99038105676658006 ) ) ;
#4135 = ORIENTED_EDGE ( 'NONE', *, *, #2870, .T. ) ;
#4136 = EDGE_LOOP ( 'NONE', ( #8783, #11844 ) ) ;
#4137 = EDGE_CURVE ( 'NONE', #8368, #10816, #7300, .T. ) ;
#4138 = CARTESIAN_POINT ( 'NONE',  ( -3.000000000000000000, 3.673940397442059868E-16, 30.00000000000000000 ) ) ;
#4139 = AXIS2_PLACEMENT_3D ( 'NONE', #6629, #2167, #13706 ) ;
#4140 = DIRECTION ( 'NONE',  ( -0.000000000000000000, -0.000000000000000000, -1.000000000000000000 ) ) ;
#4141 = PLANE ( 'NONE',  #5570 ) ;
#4142 = VERTEX_POINT ( 'NONE', #644 ) ;
#4143 = FACE_OUTER_BOUND ( 'NONE', #12077, .T. ) ;
#4144 = DIRECTION ( 'NONE',  ( 1.000000000000000000, 0.000000000000000000, -2.735665993912342121E-16 ) ) ;
#4145 = AXIS2_PLACEMENT_3D ( 'NONE', #4804, #13793, #4901 ) ;
#4146 = ADVANCED_FACE ( 'NONE', ( #15026 ), #2426, .F. ) ;
#4147 = ADVANCED_FACE ( 'NONE', ( #18091 ), #734, .F. ) ;
#4148 = CARTESIAN_POINT ( 'NONE',  ( -15.92381708198643153, -22.77559583767277473, -4.330127018922181215 ) ) ;
#4149 = PLANE ( 'NONE',  #2287 ) ;
#4150 = EDGE_CURVE ( 'NONE', #6385, #11472, #7585, .T. ) ;
#4151 = FACE_OUTER_BOUND ( 'NONE', #13087, .T. ) ;
#4152 = CARTESIAN_POINT ( 'NONE',  ( -129.1404785418517918, 9.649298036820672664, -2.500000000000007994 ) ) ;
#4153 = DIRECTION ( 'NONE',  ( -1.000000000000000000, 0.000000000000000000, 0.000000000000000000 ) ) ;
#4154 = AXIS2_PLACEMENT_3D ( 'NONE', #10823, #16537, #3901 ) ;
#4155 = VERTEX_POINT ( 'NONE', #16766 ) ;
#4156 = AXIS2_PLACEMENT_3D ( 'NONE', #5650, #11404, #13201 ) ;
#4157 = ORIENTED_EDGE ( 'NONE', *, *, #16208, .T. ) ;
#4158 = CARTESIAN_POINT ( 'NONE',  ( -32.22008523532134205, -25.36048350923618955, 12.99038105676661736 ) ) ;
#4159 = ORIENTED_EDGE ( 'NONE', *, *, #8007, .T. ) ;
#4160 = VERTEX_POINT ( 'NONE', #3730 ) ;
#4161 = VERTEX_POINT ( 'NONE', #8595 ) ;
#4162 = ORIENTED_EDGE ( 'NONE', *, *, #5404, .T. ) ;
#4163 = DIRECTION ( 'NONE',  ( 0.000000000000000000, 0.000000000000000000, 1.000000000000000000 ) ) ;
#4164 = VECTOR ( 'NONE', #460, 1000.000000000000000 ) ;
#4165 = DIRECTION ( 'NONE',  ( 1.000000000000000000, 0.000000000000000000, 0.000000000000000000 ) ) ;
#4166 = CIRCLE ( 'NONE', #1798, 1.499999999999999556 ) ;
#4167 = FACE_OUTER_BOUND ( 'NONE', #11262, .T. ) ;
#4168 = PRODUCT_DEFINITION_FORMATION_WITH_SPECIFIED_SOURCE ( 'ANY', '', #18543, .NOT_KNOWN. ) ;
#4169 = ORIENTED_EDGE ( 'NONE', *, *, #11281, .T. ) ;
#4170 = DIRECTION ( 'NONE',  ( -0.000000000000000000, -0.000000000000000000, -1.000000000000000000 ) ) ;
#4171 = EDGE_CURVE ( 'NONE', #9690, #241, #12716, .T. ) ;
#4172 = CIRCLE ( 'NONE', #12624, 1.500000000000000444 ) ;
#4173 = EDGE_CURVE ( 'NONE', #5191, #11722, #3037, .T. ) ;
#4174 = CARTESIAN_POINT ( 'NONE',  ( -19.17624791478365864, -18.22898240811121795, 8.660254037844417496 ) ) ;
#4175 = EDGE_LOOP ( 'NONE', ( #5383, #13978 ) ) ;
#4176 = ORIENTED_EDGE ( 'NONE', *, *, #5589, .F. ) ;
#4177 = ORIENTED_EDGE ( 'NONE', *, *, #5915, .T. ) ;
#4178 = DIRECTION ( 'NONE',  ( -0.1566598588826321747, 0.9876526153536343555, 0.000000000000000000 ) ) ;
#4179 = DIRECTION ( 'NONE',  ( -0.1566598588826321192, 0.9876526153536342445, 7.798540720466730171E-17 ) ) ;
#4180 = AXIS2_PLACEMENT_3D ( 'NONE', #5843, #6998, #8759 ) ;
#4181 = CARTESIAN_POINT ( 'NONE',  ( -17.69476899175320739, -17.99399261978727438, 8.660254037844417496 ) ) ;
#4182 = CIRCLE ( 'NONE', #5079, 20.00000000000001066 ) ;
#4183 = DIRECTION ( 'NONE',  ( -1.000000000000000000, 1.224646799147353207E-16, 0.000000000000000000 ) ) ;
#4184 = AXIS2_PLACEMENT_3D ( 'NONE', #3234, #12226, #2203 ) ;
#4185 = ORIENTED_EDGE ( 'NONE', *, *, #6942, .T. ) ;
#4186 = AXIS2_PLACEMENT_3D ( 'NONE', #11972, #10481, #13234 ) ;
#4187 = ORIENTED_EDGE ( 'NONE', *, *, #15526, .T. ) ;
#4188 = ORIENTED_EDGE ( 'NONE', *, *, #1246, .T. ) ;
#4189 = DIRECTION ( 'NONE',  ( 1.000000000000000000, 0.000000000000000000, 0.000000000000000000 ) ) ;
#4190 = ORIENTED_EDGE ( 'NONE', *, *, #13028, .T. ) ;
#4191 = DIRECTION ( 'NONE',  ( -0.1566598588826321192, 0.9876526153536342445, 7.798540720466730171E-17 ) ) ;
#4192 = AXIS2_PLACEMENT_3D ( 'NONE', #7334, #2666, #7140 ) ;
#4193 = DIRECTION ( 'NONE',  ( -0.000000000000000000, -0.000000000000000000, -1.000000000000000000 ) ) ;
#4194 = DIRECTION ( 'NONE',  ( -0.1566598588826321192, 0.9876526153536342445, 7.798540720466730171E-17 ) ) ;
#4195 = AXIS2_PLACEMENT_3D ( 'NONE', #4148, #2646, #6937 ) ;
#4196 = AXIS2_PLACEMENT_3D ( 'NONE', #1638, #15934, #8565 ) ;
#4197 = LINE ( 'NONE', #17214, #15685 ) ;
#4198 = CARTESIAN_POINT ( 'NONE',  ( -58.68235252892886678, -24.49537676341648407, 1.908195823574487804E-14 ) ) ;
#4199 = PRODUCT_CONTEXT ( 'NONE', #8103, 'mechanical' ) ;
#4200 = FACE_OUTER_BOUND ( 'NONE', #13986, .T. ) ;
#4201 = ORIENTED_EDGE ( 'NONE', *, *, #1480, .T. ) ;
#4202 = LINE ( 'NONE', #2798, #18071 ) ;
#4203 = CARTESIAN_POINT ( 'NONE',  ( -33.00338452973448966, -20.42222043246805896, -4.330127018922180326 ) ) ;
#4204 = ADVANCED_FACE ( 'NONE', ( #10090 ), #8393, .F. ) ;
#4205 = FACE_BOUND ( 'NONE', #985, .T. ) ;
#4206 = ORIENTED_EDGE ( 'NONE', *, *, #8271, .F. ) ;
#4207 = EDGE_CURVE ( 'NONE', #6795, #3698, #1827, .T. ) ;
#4208 = VERTEX_POINT ( 'NONE', #17231 ) ;
#4209 = DIRECTION ( 'NONE',  ( -8.693966348389027220E-17, 1.991237296706374949E-16, -1.000000000000000000 ) ) ;
#4210 = CARTESIAN_POINT ( 'NONE',  ( -85.13801595139511846, 33.83333333333333570, -30.00000000000000000 ) ) ;
#4211 = DIRECTION ( 'NONE',  ( -0.1566598588826321192, 0.9876526153536342445, 7.798540720466731404E-17 ) ) ;
#4212 = AXIS2_PLACEMENT_3D ( 'NONE', #17989, #10371, #8951 ) ;
#4213 = CIRCLE ( 'NONE', #1799, 1.500000000000000888 ) ;
#4214 = CIRCLE ( 'NONE', #16332, 1.499999999999999556 ) ;
#4215 = EDGE_LOOP ( 'NONE', ( #13219, #12560, #3284, #14554, #6804, #15849 ) ) ;
#4216 = LINE ( 'NONE', #1393, #13033 ) ;
#4217 = CARTESIAN_POINT ( 'NONE',  ( -25.26688191766807279, -81.96304593340587985, -21.65063509461098690 ) ) ;
#4219 = CARTESIAN_POINT ( 'NONE',  ( -129.1237011781999513, 8.819295008908911271, 5.132545408516866914 ) ) ;
#4218 = CIRCLE ( 'NONE', #287, 1.500000000000000888 ) ;
#4220 = VECTOR ( 'NONE', #15086, 1000.000000000000000 ) ;
#4221 = DIRECTION ( 'NONE',  ( -0.9876526153536341335, -0.1566598588826327021, 0.000000000000000000 ) ) ;
#4222 = CARTESIAN_POINT ( 'NONE',  ( -69.25705831108246002, -31.23522821733487476, -8.660254037844380193 ) ) ;
#4223 = SURFACE_STYLE_FILL_AREA ( #9827 ) ;
#4224 = EDGE_LOOP ( 'NONE', ( #3666, #13144 ) ) ;
#4225 = CIRCLE ( 'NONE', #9701, 1.500000000000001332 ) ;
#4226 =( REPRESENTATION_RELATIONSHIP ('NONE','NONE', #7353, #13723 ) REPRESENTATION_RELATIONSHIP_WITH_TRANSFORMATION ( #5548 )SHAPE_REPRESENTATION_RELATIONSHIP( ) );
#4227 = CARTESIAN_POINT ( 'NONE',  ( -59.83472345504510770, -87.44614099429797704, -21.65063509461098690 ) ) ;
#4228 = AXIS2_PLACEMENT_3D ( 'NONE', #514, #9143, #14913 ) ;
#4229 = LINE ( 'NONE', #8779, #12300 ) ;
#4230 = CARTESIAN_POINT ( 'NONE',  ( -55.42992169613163611, -29.04199019297804085, -21.65063509461098334 ) ) ;
#4231 = CARTESIAN_POINT ( 'NONE',  ( 5.005906274354426217E-15, -2.199999999999998845, -20.00000000000000355 ) ) ;
#4232 = ORIENTED_EDGE ( 'NONE', *, *, #15098, .F. ) ;
#4233 = VERTEX_POINT ( 'NONE', #17332 ) ;
#4234 = DIRECTION ( 'NONE',  ( -0.1566598588826321747, 0.9876526153536343555, 0.000000000000000000 ) ) ;
#4235 = CARTESIAN_POINT ( 'NONE',  ( -76.88766983611584749, -2.536636612185957595, 7.500000000000000000 ) ) ;
#4237 = ORIENTED_EDGE ( 'NONE', *, *, #13563, .T. ) ;
#4236 = DIRECTION ( 'NONE',  ( -0.1566598588826321192, 0.9876526153536342445, 7.798540720466731404E-17 ) ) ;
#4238 = AXIS2_PLACEMENT_3D ( 'NONE', #3751, #16880, #8330 ) ;
#4239 = ORIENTED_EDGE ( 'NONE', *, *, #10939, .F. ) ;
#4240 = EDGE_LOOP ( 'NONE', ( #13373, #1217 ) ) ;
#4241 = EDGE_CURVE ( 'NONE', #14450, #7294, #18538, .T. ) ;
#4242 = CARTESIAN_POINT ( 'NONE',  ( -17.40529600501688279, -23.01058562599671831, 12.99038105676661381 ) ) ;
#4243 = CIRCLE ( 'NONE', #7576, 13.99999999999999822 ) ;
#4244 = ORIENTED_EDGE ( 'NONE', *, *, #13023, .F. ) ;
#4245 = VECTOR ( 'NONE', #14138, 1000.000000000000000 ) ;
#4246 = CIRCLE ( 'NONE', #8508, 1.500000000000000888 ) ;
#4247 = DIRECTION ( 'NONE',  ( -0.1566598588826321192, 0.9876526153536342445, 7.798540720466730171E-17 ) ) ;
#4248 = ADVANCED_FACE ( 'NONE', ( #1308 ), #14457, .F. ) ;
#4249 = DIRECTION ( 'NONE',  ( 0.000000000000000000, 0.000000000000000000, 1.000000000000000000 ) ) ;
#4250 = CYLINDRICAL_SURFACE ( 'NONE', #1334, 2.200000000000000178 ) ;
#4251 = CARTESIAN_POINT ( 'NONE',  ( -67.57122606711153878, -25.90531549336015971, -21.65063509461098334 ) ) ;
#4252 = DIRECTION ( 'NONE',  ( -0.9876526153536336894, -0.1566598588826349503, 0.000000000000000000 ) ) ;
#4253 = ORIENTED_EDGE ( 'NONE', *, *, #10939, .T. ) ;
#4254 = CIRCLE ( 'NONE', #13336, 1.500000000000000444 ) ;
#4255 = LINE ( 'NONE', #8540, #1780 ) ;
#4256 = AXIS2_PLACEMENT_3D ( 'NONE', #732, #8958, #16371 ) ;
#4257 = CARTESIAN_POINT ( 'NONE',  ( -29.21749237908258223, -82.58968536893642920, 17.32050807568881368 ) ) ;
#4258 = FACE_BOUND ( 'NONE', #10149, .T. ) ;
#4259 = CYLINDRICAL_SURFACE ( 'NONE', #1006, 1.500000000000001554 ) ;
#4260 = CIRCLE ( 'NONE', #1842, 1.500000000000000000 ) ;
#4261 = CARTESIAN_POINT ( 'NONE',  ( -20.86208015875458344, -23.55889513208593655, 12.99038105676661736 ) ) ;
#4262 = DIRECTION ( 'NONE',  ( -0.1566598588826321192, 0.9876526153536342445, 7.798540720466730171E-17 ) ) ;
#4263 = ORIENTED_EDGE ( 'NONE', *, *, #5442, .F. ) ;
#4264 = ORIENTED_EDGE ( 'NONE', *, *, #15989, .T. ) ;
#4265 = FACE_OUTER_BOUND ( 'NONE', #2447, .T. ) ;
#4266 = EDGE_CURVE ( 'NONE', #12815, #15547, #1215, .T. ) ;
#4267 = ORIENTED_EDGE ( 'NONE', *, *, #11314, .F. ) ;
#4268 = EDGE_LOOP ( 'NONE', ( #2639, #8226 ) ) ;
#4269 = CARTESIAN_POINT ( 'NONE',  ( -10.78120068427780964, -16.89737360760884144, -17.32050807568878170 ) ) ;
#4270 = B_SPLINE_CURVE_WITH_KNOTS ( 'NONE', 3,
 ( #16744, #13757, #9518, #13857, #13964, #12529, #14053, #2124, #16635, #18285, #7912, #13672, #18374, #3892, #9722, #1099, #4385, #18664 ),
 .UNSPECIFIED., .F., .F.,
 ( 4, 2, 2, 2, 2, 2, 2, 2, 4 ),
 ( 1.734723475976807094E-18, 0.0006036110467294001801, 0.001207222093458798625, 0.001810833140188197179, 0.002414444186917595516, 0.003018055233646994937, 0.003621666280376394792, 0.004225277327105794213, 0.004828888373835193634 ),
 .UNSPECIFIED. ) ;
#4271 = CIRCLE ( 'NONE', #9648, 1.500000000000001332 ) ;
#4272 = FACE_BOUND ( 'NONE', #9666, .T. ) ;
#4273 = EDGE_CURVE ( 'NONE', #12329, #886, #2704, .T. ) ;
#4274 = DIRECTION ( 'NONE',  ( 0.000000000000000000, 0.000000000000000000, 1.000000000000000000 ) ) ;
#4275 = AXIS2_PLACEMENT_3D ( 'NONE', #14532, #11650, #14253 ) ;
#4276 = DIRECTION ( 'NONE',  ( 1.000000000000000000, 0.000000000000000000, 0.000000000000000000 ) ) ;
#4277 = EDGE_LOOP ( 'NONE', ( #9126, #1921, #3542, #12695 ) ) ;
#4278 = CIRCLE ( 'NONE', #17017, 2.000000000000001776 ) ;
#4279 = CARTESIAN_POINT ( 'NONE',  ( -85.86167379012967160, 34.32252072304513746, 35.00000000000000000 ) ) ;
#4280 = VERTEX_POINT ( 'NONE', #285 ) ;
#4281 = VECTOR ( 'NONE', #9561, 1000.000000000000000 ) ;
#4282 = AXIS2_PLACEMENT_3D ( 'NONE', #11392, #17215, #6397 ) ;
#4283 = LINE ( 'NONE', #1363, #9403 ) ;
#4285 = EDGE_CURVE ( 'NONE', #9461, #7705, #15151, .T. ) ;
#4284 = CYLINDRICAL_SURFACE ( 'NONE', #9987, 1.500000000000000888 ) ;
#4286 = DIRECTION ( 'NONE',  ( 0.000000000000000000, 0.000000000000000000, 1.000000000000000000 ) ) ;
#4287 = CIRCLE ( 'NONE', #14285, 1.500000000000000444 ) ;
#4289 = EDGE_LOOP ( 'NONE', ( #7155, #3052 ) ) ;
#4288 = EDGE_CURVE ( 'NONE', #294, #3396, #5891, .T. ) ;
#4290 = VERTEX_POINT ( 'NONE', #17842 ) ;
#4291 = EDGE_LOOP ( 'NONE', ( #12304, #12229, #16969, #10131 ) ) ;
#4292 = CARTESIAN_POINT ( 'NONE',  ( -16.87183468716221313, -80.63143713290352821, -4.330127018922185655 ) ) ;
#4293 = EDGE_CURVE ( 'NONE', #15166, #18004, #7010, .T. ) ;
#4294 = EDGE_CURVE ( 'NONE', #12874, #10229, #13927, .T. ) ;
#4295 = ORIENTED_EDGE ( 'NONE', *, *, #12442, .T. ) ;
#4296 = FACE_BOUND ( 'NONE', #13349, .T. ) ;
#4297 = EDGE_CURVE ( 'NONE', #16444, #4718, #2754, .T. ) ;
#4298 = DIRECTION ( 'NONE',  ( -0.1566598588826321747, 0.9876526153536343555, 0.000000000000000000 ) ) ;
#4299 = ORIENTED_EDGE ( 'NONE', *, *, #10177, .F. ) ;
#4300 = DIRECTION ( 'NONE',  ( -0.1566598588826321192, 0.9876526153536342445, 7.798540720466730171E-17 ) ) ;
#4301 = DIRECTION ( 'NONE',  ( 1.000000000000000000, 0.000000000000000000, -0.000000000000000000 ) ) ;
#4302 = CIRCLE ( 'NONE', #14888, 1.499999999999999556 ) ;
#4303 = DIRECTION ( 'NONE',  ( 0.000000000000000000, 0.000000000000000000, 1.000000000000000000 ) ) ;
#4304 = ITEM_DEFINED_TRANSFORMATION ( 'NONE', 'NONE', #4154,  #18772 ) ;
#4305 = CARTESIAN_POINT ( 'NONE',  ( 1.893565004556770903, -77.65489981413351472, 1.096166233436304165E-14 ) ) ;
#4306 = DIRECTION ( 'NONE',  ( 0.000000000000000000, 0.000000000000000000, 1.000000000000000000 ) ) ;
#4307 = AXIS2_PLACEMENT_3D ( 'NONE', #4829, #18044, #9389 ) ;
#4308 = CARTESIAN_POINT ( 'NONE',  ( -70.00000000000001421, 44.99999999999998579, -7.500000000000000000 ) ) ;
#4309 = ORIENTED_EDGE ( 'NONE', *, *, #1871, .F. ) ;
#4310 = VERTEX_POINT ( 'NONE', #15244 ) ;
#4311 = CARTESIAN_POINT ( 'NONE',  ( -71.02801022084922522, -26.45362499944937440, -12.99038105676658006 ) ) ;
#4312 = DIRECTION ( 'NONE',  ( -0.9876526153536341335, -0.1566598588826327576, 0.000000000000000000 ) ) ;
#4313 = DIRECTION ( 'NONE',  ( 0.000000000000000000, 0.000000000000000000, 1.000000000000000000 ) ) ;
#4314 = EDGE_CURVE ( 'NONE', #6912, #5315, #9405, .T. ) ;
#4315 = ADVANCED_FACE ( 'NONE', ( #7866 ), #6462, .F. ) ;
#4316 = CIRCLE ( 'NONE', #14615, 1.500000000000000000 ) ;
#4317 = ORIENTED_EDGE ( 'NONE', *, *, #6276, .T. ) ;
#4318 = ORIENTED_EDGE ( 'NONE', *, *, #4629, .F. ) ;
#4319 = CARTESIAN_POINT ( 'NONE',  ( -63.78533391645962780, -88.07278042982854060, 17.32050807568881368 ) ) ;
#4320 = EDGE_LOOP ( 'NONE', ( #4636, #8294 ) ) ;
#4321 = EDGE_CURVE ( 'NONE', #7992, #7156, #3388, .T. ) ;
#4322 = CYLINDRICAL_SURFACE ( 'NONE', #17916, 1.500000000000001554 ) ;
#4323 = CARTESIAN_POINT ( 'NONE',  ( -18.39294862037050393, -23.16724548487935564, 1.869203119972154228E-14 ) ) ;
#4324 = CARTESIAN_POINT ( 'NONE',  ( -66.78792677269838407, -30.84357857012830095, -4.330127018922181215 ) ) ;
#4325 = ORIENTED_EDGE ( 'NONE', *, *, #16497, .F. ) ;
#4326 = AXIS2_PLACEMENT_3D ( 'NONE', #10608, #16209, #17747 ) ;
#4327 = DIRECTION ( 'NONE',  ( -0.9876526153536336894, -0.1566598588826349503, 0.000000000000000000 ) ) ;
#4328 = CARTESIAN_POINT ( 'NONE',  ( -65.23030399291525327, 43.49999999999997868, -19.99999999999999645 ) ) ;
#4329 = DIRECTION ( 'NONE',  ( -0.9876526153536336894, -0.1566598588826349503, 0.000000000000000000 ) ) ;
#4330 = CARTESIAN_POINT ( 'NONE',  ( -53.94844277310117064, -28.80700040465408662, 4.330127018922217630 ) ) ;
#4331 = DIRECTION ( 'NONE',  ( 0.000000000000000000, 0.000000000000000000, 1.000000000000000000 ) ) ;
#4333 = VERTEX_POINT ( 'NONE', #3758 ) ;
#4332 = DIRECTION ( 'NONE',  ( -0.9876526153536341335, -0.1566598588826327021, 0.000000000000000000 ) ) ;
#4334 = ORIENTED_EDGE ( 'NONE', *, *, #11593, .F. ) ;
#4335 = ORIENTED_EDGE ( 'NONE', *, *, #11679, .F. ) ;
#4336 = CARTESIAN_POINT ( 'NONE',  ( -66.25446545484369665, -88.46443007703510375, -21.65063509461098690 ) ) ;
#4337 = ORIENTED_EDGE ( 'NONE', *, *, #3578, .T. ) ;
#4338 = AXIS2_PLACEMENT_3D ( 'NONE', #3933, #2441, #7841 ) ;
#4339 = DIRECTION ( 'NONE',  ( 1.224646799147353207E-16, 1.000000000000000000, -0.000000000000000000 ) ) ;
#4340 = EDGE_CURVE ( 'NONE', #12777, #11183, #13325, .T. ) ;
#4341 = DIRECTION ( 'NONE',  ( -1.000000000000000000, 0.000000000000000000, 0.000000000000000000 ) ) ;
#4342 =( REPRESENTATION_RELATIONSHIP ('NONE','NONE', #7353, #13127 ) REPRESENTATION_RELATIONSHIP_WITH_TRANSFORMATION ( #4304 )SHAPE_REPRESENTATION_RELATIONSHIP( ) );
#4343 = EDGE_CURVE ( 'NONE', #6457, #2469, #16587, .T. ) ;
#4344 = CYLINDRICAL_SURFACE ( 'NONE', #16775, 1.500000000000001554 ) ;
#4345 = ORIENTED_EDGE ( 'NONE', *, *, #10580, .F. ) ;
#4346 = FACE_OUTER_BOUND ( 'NONE', #13527, .T. ) ;
#4347 = DIRECTION ( 'NONE',  ( -0.1566598588826321192, 0.9876526153536342445, 7.798540720466730171E-17 ) ) ;
#4348 = ADVANCED_FACE ( 'NONE', ( #10873 ), #16696, .F. ) ;
#4349 = CARTESIAN_POINT ( 'NONE',  ( -24.31886431249228053, -24.10720463817513703, -4.330127018922181215 ) ) ;
#4350 = ORIENTED_EDGE ( 'NONE', *, *, #1649, .T. ) ;
#4351 = CARTESIAN_POINT ( 'NONE',  ( 0.000000000000000000, 0.000000000000000000, -35.00000000000000000 ) ) ;
#4352 = DIRECTION ( 'NONE',  ( -0.1566598588826321192, 0.9876526153536342445, 7.798540720466730171E-17 ) ) ;
#4354 = EDGE_LOOP ( 'NONE', ( #12014, #17117 ) ) ;
#4353 = AXIS2_PLACEMENT_3D ( 'NONE', #8401, #8507, #2529 ) ;
#4355 = ORIENTED_EDGE ( 'NONE', *, *, #15048, .F. ) ;
#4356 = ORIENTED_EDGE ( 'NONE', *, *, #12590, .T. ) ;
#4357 = ORIENTED_EDGE ( 'NONE', *, *, #15152, .T. ) ;
#4358 = DIRECTION ( 'NONE',  ( -0.9876526153536341335, -0.1566598588826327021, 0.000000000000000000 ) ) ;
#4359 = VERTEX_POINT ( 'NONE', #9276 ) ;
#4360 = DIRECTION ( 'NONE',  ( -0.9876526153536336894, -0.1566598588826349503, 0.000000000000000000 ) ) ;
#4361 = ORIENTED_EDGE ( 'NONE', *, *, #18102, .F. ) ;
#4362 = VERTEX_POINT ( 'NONE', #13634 ) ;
#4363 = CARTESIAN_POINT ( 'NONE',  ( -173.0810787726268245, 56.45151975169577696, 2.500000000000000000 ) ) ;
#4364 = CARTESIAN_POINT ( 'NONE',  ( -51.27495791377663181, -23.32042782179674489, -4.330127018922180326 ) ) ;
#4365 = DIRECTION ( 'NONE',  ( -0.1566598588826321192, 0.9876526153536342445, 7.798540720466731404E-17 ) ) ;
#4366 = ORIENTED_EDGE ( 'NONE', *, *, #9124, .T. ) ;
#4367 = EDGE_CURVE ( 'NONE', #12785, #3795, #3934, .T. ) ;
#4368 = DIRECTION ( 'NONE',  ( -0.000000000000000000, -0.000000000000000000, -1.000000000000000000 ) ) ;
#4369 = EDGE_LOOP ( 'NONE', ( #7507, #5555 ) ) ;
#4370 = DIRECTION ( 'NONE',  ( -0.9710487832595061652, 0.2388812686885108671, 0.000000000000000000 ) ) ;
#4371 = DIRECTION ( 'NONE',  ( 0.000000000000000000, 0.000000000000000000, 1.000000000000000000 ) ) ;
#4372 = FACE_OUTER_BOUND ( 'NONE', #18179, .T. ) ;
#4374 = EDGE_CURVE ( 'NONE', #5969, #18512, #2549, .T. ) ;
#4373 = CARTESIAN_POINT ( 'NONE',  ( -21.64537945316773460, -18.62063205531779175, -21.65063509461097979 ) ) ;
#4375 = FACE_BOUND ( 'NONE', #16095, .T. ) ;
#4376 = CARTESIAN_POINT ( 'NONE',  ( -8.516422466834198346, -21.60064689605303911, 17.32050807568881012 ) ) ;
#4377 = ORIENTED_EDGE ( 'NONE', *, *, #15869, .T. ) ;
#4378 = EDGE_LOOP ( 'NONE', ( #9533, #10 ) ) ;
#4379 = VERTEX_POINT ( 'NONE', #4615 ) ;
#4380 = VERTEX_POINT ( 'NONE', #11703 ) ;
#4381 = DIRECTION ( 'NONE',  ( 0.000000000000000000, 1.000000000000000000, 1.224646799147353207E-16 ) ) ;
#4382 = VERTEX_POINT ( 'NONE', #3009 ) ;
#4383 = VECTOR ( 'NONE', #5984, 1000.000000000000000 ) ;
#4384 = FACE_BOUND ( 'NONE', #4033, .T. ) ;
#4385 = CARTESIAN_POINT ( 'NONE',  ( -170.5817629592740730, 32.44593076567889511, 5.316127001577102718 ) ) ;
#4386 = DIRECTION ( 'NONE',  ( 0.000000000000000000, 0.000000000000000000, 1.000000000000000000 ) ) ;
#4387 = CONTEXT_DEPENDENT_SHAPE_REPRESENTATION ( #9073, #7879 ) ;
#4388 = ADVANCED_FACE ( 'NONE', ( #6055 ), #13332, .F. ) ;
#4389 = EDGE_CURVE ( 'NONE', #6775, #16721, #15902, .T. ) ;
#4390 = CARTESIAN_POINT ( 'NONE',  ( -174.8056419950568738, 55.54559466234915277, 4.582591203971079885 ) ) ;
#4391 = VECTOR ( 'NONE', #13402, 1000.000000000000000 ) ;
#4392 = DIRECTION ( 'NONE',  ( -0.1566598588826321192, 0.9876526153536342445, 7.798540720466731404E-17 ) ) ;
#4393 = EDGE_CURVE ( 'NONE', #15929, #18110, #7595, .T. ) ;
#4394 = DIRECTION ( 'NONE',  ( -0.1566598588826321192, 0.9876526153536342445, 7.798540720466731404E-17 ) ) ;
#4395 = DIRECTION ( 'NONE',  ( 0.000000000000000000, 0.000000000000000000, 1.000000000000000000 ) ) ;
#4396 = FACE_OUTER_BOUND ( 'NONE', #1097, .T. ) ;
#4397 = ORIENTED_EDGE ( 'NONE', *, *, #564, .F. ) ;
#4398 = VERTEX_POINT ( 'NONE', #18605 ) ;
#4399 = DIRECTION ( 'NONE',  ( -0.000000000000000000, -0.000000000000000000, -1.000000000000000000 ) ) ;
#4400 = VERTEX_POINT ( 'NONE', #8509 ) ;
#4401 = DIRECTION ( 'NONE',  ( -0.1566598588826321747, 0.9876526153536343555, 0.000000000000000000 ) ) ;
#4402 = DIRECTION ( 'NONE',  ( 0.000000000000000000, 0.000000000000000000, 1.000000000000000000 ) ) ;
#4403 = VERTEX_POINT ( 'NONE', #8124 ) ;
#4404 = DIRECTION ( 'NONE',  ( -0.9876526153536336894, -0.1566598588826349503, 0.000000000000000000 ) ) ;
#4405 = AXIS2_PLACEMENT_3D ( 'NONE', #1571, #17325, #16154 ) ;
#4406 = DIRECTION ( 'NONE',  ( -0.9876526153536336894, -0.1566598588826349503, 0.000000000000000000 ) ) ;
#4407 = ORIENTED_EDGE ( 'NONE', *, *, #17051, .T. ) ;
#4408 = ADVANCED_FACE ( 'NONE', ( #1129 ), #12646, .T. ) ;
#4409 = VECTOR ( 'NONE', #18457, 1000.000000000000000 ) ;
#4410 = CARTESIAN_POINT ( 'NONE',  ( -2.000000000000000000, 0.000000000000000000, -30.00000000000000000 ) ) ;
#4411 = DIRECTION ( 'NONE',  ( 1.000000000000000000, 0.000000000000000000, -2.631994239413086031E-16 ) ) ;
#4412 = CARTESIAN_POINT ( 'NONE',  ( -31.68662391746666884, -82.98133501614299234, -12.99038105676658539 ) ) ;
#4413 = CARTESIAN_POINT ( 'NONE',  ( -309.1404785418517918, -2.850701963179328668, 12.83663829214476237 ) ) ;
#4414 = EDGE_LOOP ( 'NONE', ( #7322, #6758 ) ) ;
#4415 = EDGE_LOOP ( 'NONE', ( #12895, #501, #15641, #9969 ) ) ;
#4416 = DIRECTION ( 'NONE',  ( 1.000000000000000000, 0.000000000000000000, 0.000000000000000000 ) ) ;
#4417 = CIRCLE ( 'NONE', #2608, 2.000000000000000000 ) ;
#4419 = VERTEX_POINT ( 'NONE', #1587 ) ;
#4418 = DIRECTION ( 'NONE',  ( -0.9876526153536341335, -0.1566598588826327021, 0.000000000000000000 ) ) ;
#4420 = ORIENTED_EDGE ( 'NONE', *, *, #4028, .F. ) ;
#4421 = VECTOR ( 'NONE', #5232, 1000.000000000000000 ) ;
#4422 = CARTESIAN_POINT ( 'NONE',  ( 5.000000000000004441, 6.123233995736772199E-16, -20.00000000000000355 ) ) ;
#4423 = FACE_OUTER_BOUND ( 'NONE', #3034, .T. ) ;
#4424 = DIRECTION ( 'NONE',  ( 0.000000000000000000, 0.000000000000000000, 1.000000000000000000 ) ) ;
#4425 = CARTESIAN_POINT ( 'NONE',  ( -49.95819730150881099, -85.87954240547166762, -21.65063509461098690 ) ) ;
#4426 = CIRCLE ( 'NONE', #11670, 1.499999999999999556 ) ;
#4427 = CARTESIAN_POINT ( 'NONE',  ( -15.88418207180859021, -80.47477727402089442, -8.660254037844385522 ) ) ;
#4428 = LINE ( 'NONE', #15828, #2360 ) ;
#4429 = CARTESIAN_POINT ( 'NONE',  ( -56.21322099054479082, -24.10372711620989605, -21.65063509461097979 ) ) ;
#4430 = ORIENTED_EDGE ( 'NONE', *, *, #1045, .T. ) ;
#4431 = CARTESIAN_POINT ( 'NONE',  ( 1.893565004556770903, -77.65489981413351472, -8.660254037844385522 ) ) ;
#4432 = AXIS2_PLACEMENT_3D ( 'NONE', #14024, #9772, #9938 ) ;
#4433 = CARTESIAN_POINT ( 'NONE',  ( -13.41505053342451426, -80.08312762681433128, -4.330127018922185655 ) ) ;
#4434 = CARTESIAN_POINT ( 'NONE',  ( -126.1404785418517918, 9.595891400605989219, -2.500000000000000000 ) ) ;
#4436 = VERTEX_POINT ( 'NONE', #7369 ) ;
#4435 = CARTESIAN_POINT ( 'NONE',  ( -306.0881213225399051, -2.850701963179328668, 9.951701414186818625E-16 ) ) ;
#4437 = EDGE_CURVE ( 'NONE', #15703, #17521, #4260, .T. ) ;
#4438 = EDGE_LOOP ( 'NONE', ( #10812, #3149, #8903, #13669 ) ) ;
#4439 = EDGE_CURVE ( 'NONE', #18049, #5889, #4596, .T. ) ;
#4440 = LINE ( 'NONE', #3024, #11684 ) ;
#4441 = AXIS2_PLACEMENT_3D ( 'NONE', #725, #16651, #6508 ) ;
#4442 = ORIENTED_EDGE ( 'NONE', *, *, #12055, .F. ) ;
#4443 = CIRCLE ( 'NONE', #2028, 1.500000000000000888 ) ;
#4444 = ORIENTED_EDGE ( 'NONE', *, *, #5295, .T. ) ;
#4445 = DIRECTION ( 'NONE',  ( -0.1566598588826321192, 0.9876526153536342445, 7.798540720466730171E-17 ) ) ;
#4446 = EDGE_CURVE ( 'NONE', #10913, #2476, #17311, .T. ) ;
#4447 = AXIS2_PLACEMENT_3D ( 'NONE', #3735, #3825, #4890 ) ;
#4448 = FACE_BOUND ( 'NONE', #2249, .T. ) ;
#4449 = ORIENTED_EDGE ( 'NONE', *, *, #10314, .T. ) ;
#4450 = CARTESIAN_POINT ( 'NONE',  ( -42.87991068327077926, -21.98881902129437549, -4.330127018922180326 ) ) ;
#4451 = ORIENTED_EDGE ( 'NONE', *, *, #2660, .T. ) ;
#4452 =( GEOMETRIC_REPRESENTATION_CONTEXT ( 3 ) GLOBAL_UNCERTAINTY_ASSIGNED_CONTEXT ( ( #5444 ) ) GLOBAL_UNIT_ASSIGNED_CONTEXT ( ( #4502, #6419, #10283 ) ) REPRESENTATION_CONTEXT ( 'NONE', 'WORKASPACE' ) );
#4453 = ORIENTED_EDGE ( 'NONE', *, *, #4573, .F. ) ;
#4454 = FACE_BOUND ( 'NONE', #5287, .T. ) ;
#4456 = ORIENTED_EDGE ( 'NONE', *, *, #14274, .F. ) ;
#4455 = AXIS2_PLACEMENT_3D ( 'NONE', #2180, #3208, #9104 ) ;
#4457 =( NAMED_UNIT ( * ) SI_UNIT ( $, .STERADIAN. ) SOLID_ANGLE_UNIT ( ) );
#4458 = LINE ( 'NONE', #1278, #13621 ) ;
#4459 = LINE ( 'NONE', #9182, #8788 ) ;
#4460 = CYLINDRICAL_SURFACE ( 'NONE', #4196, 1.500000000000000666 ) ;
#4461 = AXIS2_PLACEMENT_3D ( 'NONE', #7220, #16682, #10684 ) ;
#4462 = CYLINDRICAL_SURFACE ( 'NONE', #8748, 1.500000000000001554 ) ;
#4463 = VERTEX_POINT ( 'NONE', #11677 ) ;
#4464 = EDGE_LOOP ( 'NONE', ( #18502, #1164, #4687, #10917 ) ) ;
#4465 = ORIENTED_EDGE ( 'NONE', *, *, #3350, .T. ) ;
#4466 = EDGE_LOOP ( 'NONE', ( #4740, #8137, #4584, #3204 ) ) ;
#4467 = VERTEX_POINT ( 'NONE', #5931 ) ;
#4468 = CARTESIAN_POINT ( 'NONE',  ( -12.75650591498505371, -17.21069332537411256, 1.926565525561698076E-14 ) ) ;
#4469 = EDGE_CURVE ( 'NONE', #10372, #12073, #153, .T. ) ;
#4470 = ORIENTED_EDGE ( 'NONE', *, *, #16230, .T. ) ;
#4471 = FACE_BOUND ( 'NONE', #6433, .T. ) ;
#4472 = AXIS2_PLACEMENT_3D ( 'NONE', #5791, #1339, #11705 ) ;
#4473 = DIRECTION ( 'NONE',  ( -0.000000000000000000, -0.000000000000000000, -1.000000000000000000 ) ) ;
#4474 = EDGE_CURVE ( 'NONE', #6623, #4333, #15770, .T. ) ;
#4475 = CIRCLE ( 'NONE', #15942, 1.500000000000000888 ) ;
#4476 = EDGE_LOOP ( 'NONE', ( #17899, #1840, #16199, #5121 ) ) ;
#4477 = AXIS2_PLACEMENT_3D ( 'NONE', #228, #3338, #3152 ) ;
#4478 = FACE_BOUND ( 'NONE', #17233, .T. ) ;
#4479 = CIRCLE ( 'NONE', #557, 1.499999999999999556 ) ;
#4480 = VECTOR ( 'NONE', #6702, 1000.000000000000000 ) ;
#4481 = CARTESIAN_POINT ( 'NONE',  ( -29.05277406831996245, -19.79558099693754158, 17.32050807568882078 ) ) ;
#4482 = CARTESIAN_POINT ( 'NONE',  ( -174.6915139316591024, 55.69864286368945017, 4.224609204322596234 ) ) ;
#4483 = DIRECTION ( 'NONE',  ( -0.1566598588826321747, 0.9876526153536343555, 0.000000000000000000 ) ) ;
#4484 =( GEOMETRIC_REPRESENTATION_CONTEXT ( 3 ) GLOBAL_UNCERTAINTY_ASSIGNED_CONTEXT ( ( #3573 ) ) GLOBAL_UNIT_ASSIGNED_CONTEXT ( ( #744, #5284, #18405 ) ) REPRESENTATION_CONTEXT ( 'NONE', 'WORKASPACE' ) );
#4485 = CARTESIAN_POINT ( 'NONE',  ( -81.73462711737164454, 33.01666666666666572, 30.00000000000000000 ) ) ;
#4486 = CARTESIAN_POINT ( 'NONE',  ( -174.8047394602870384, 55.54704694713838364, -4.579216830445309583 ) ) ;
#4487 = FACE_BOUND ( 'NONE', #12157, .T. ) ;
#4488 = VERTEX_POINT ( 'NONE', #68 ) ;
#4489 = EDGE_LOOP ( 'NONE', ( #15605, #13376, #4659, #17869 ) ) ;
#4490 = DIRECTION ( 'NONE',  ( -0.9876526153536341335, -0.1566598588826327021, 0.000000000000000000 ) ) ;
#4491 = DIRECTION ( 'NONE',  ( -0.1566598588826321192, 0.9876526153536342445, 7.798540720466730171E-17 ) ) ;
#4492 = ORIENTED_EDGE ( 'NONE', *, *, #5044, .F. ) ;
#4493 = EDGE_CURVE ( 'NONE', #13102, #17604, #15719, .T. ) ;
#4494 = CIRCLE ( 'NONE', #17835, 149.4844750268701148 ) ;
#4495 = ORIENTED_EDGE ( 'NONE', *, *, #6919, .F. ) ;
#4496 = DIRECTION ( 'NONE',  ( -0.000000000000000000, -0.000000000000000000, -1.000000000000000000 ) ) ;
#4497 = EDGE_LOOP ( 'NONE', ( #6515, #13015 ) ) ;
#4498 = VECTOR ( 'NONE', #10905, 1000.000000000000000 ) ;
#4499 = ADVANCED_FACE ( 'NONE', ( #15802 ), #6026, .F. ) ;
#4500 = DIRECTION ( 'NONE',  ( 0.000000000000000000, 0.000000000000000000, 1.000000000000000000 ) ) ;
#4501 = DIRECTION ( 'NONE',  ( 0.000000000000000000, 0.000000000000000000, 1.000000000000000000 ) ) ;
#4502 =( LENGTH_UNIT ( ) NAMED_UNIT ( * ) SI_UNIT ( .MILLI., .METRE. ) );
#4503 = CARTESIAN_POINT ( 'NONE',  ( -54.73174206751433957, -23.86873732788595248, -21.65063509461098334 ) ) ;
#4505 = CARTESIAN_POINT ( 'NONE',  ( -43.86756329862440396, -22.14547888017701638, 17.32050807568882078 ) ) ;
#4504 = CIRCLE ( 'NONE', #6954, 1.500000000000000888 ) ;
#4506 = DIRECTION ( 'NONE',  ( -0.1566598588826321192, 0.9876526153536342445, 7.798540720466730171E-17 ) ) ;
#4507 = DIRECTION ( 'NONE',  ( 0.000000000000000000, 0.000000000000000000, 1.000000000000000000 ) ) ;
#4508 = ORIENTED_EDGE ( 'NONE', *, *, #8569, .F. ) ;
#4509 = CARTESIAN_POINT ( 'NONE',  ( 0.000000000000000000, 0.000000000000000000, 20.00000000000000000 ) ) ;
#4510 = AXIS2_PLACEMENT_3D ( 'NONE', #4873, #3252, #6321 ) ;
#4511 = EDGE_LOOP ( 'NONE', ( #7483, #18589, #4964, #2663 ) ) ;
#4512 = CARTESIAN_POINT ( 'NONE',  ( -55.42992169613163611, -29.04199019297804085, -21.65063509461098334 ) ) ;
#4513 = ORIENTED_EDGE ( 'NONE', *, *, #16228, .T. ) ;
#4514 = EDGE_CURVE ( 'NONE', #3138, #6411, #10096, .T. ) ;
#4515 = ADVANCED_FACE ( 'NONE', ( #12928 ), #10370, .F. ) ;
#4516 = EDGE_CURVE ( 'NONE', #10603, #8941, #8765, .T. ) ;
#4517 = CIRCLE ( 'NONE', #7547, 1.500000000000000888 ) ;
#4518 = CARTESIAN_POINT ( 'NONE',  ( -34.97868976044173195, -20.73554015023332653, -4.330127018922180326 ) ) ;
#4519 = EDGE_LOOP ( 'NONE', ( #17371, #5776 ) ) ;
#4520 = CIRCLE ( 'NONE', #18509, 1.499999999999999556 ) ;
#4521 = CYLINDRICAL_SURFACE ( 'NONE', #13942, 1.500000000000001554 ) ;
#4522 = DIRECTION ( 'NONE',  ( -0.1566598588826321747, 0.9876526153536343555, 0.000000000000000000 ) ) ;
#4523 = CIRCLE ( 'NONE', #17270, 1.500000000000001332 ) ;
#4524 = AXIS2_PLACEMENT_3D ( 'NONE', #2304, #15491, #18289 ) ;
#4525 = CARTESIAN_POINT ( 'NONE',  ( -45.34904222165485521, -22.38046866850095640, 1.908195823574487804E-14 ) ) ;
#4526 = FACE_OUTER_BOUND ( 'NONE', #13773, .T. ) ;
#4527 = DIRECTION ( 'NONE',  ( -0.000000000000000000, -0.000000000000000000, -1.000000000000000000 ) ) ;
#4528 = ORIENTED_EDGE ( 'NONE', *, *, #149, .F. ) ;
#4529 = DIRECTION ( 'NONE',  ( -0.1566598588826321192, 0.9876526153536342445, 7.798540720466730171E-17 ) ) ;
#4530 = FACE_BOUND ( 'NONE', #4175, .T. ) ;
#4531 = VECTOR ( 'NONE', #6232, 1000.000000000000000 ) ;
#4532 = DIRECTION ( 'NONE',  ( -0.1566598588826321747, 0.9876526153536343555, 0.000000000000000000 ) ) ;
#4533 = LINE ( 'NONE', #8005, #11464 ) ;
#4534 = AXIS2_PLACEMENT_3D ( 'NONE', #14999, #4483, #13287 ) ;
#4535 = CARTESIAN_POINT ( 'NONE',  ( -66.78792677269838407, -30.84357857012830095, -21.65063509461098334 ) ) ;
#4537 = ORIENTED_EDGE ( 'NONE', *, *, #224, .T. ) ;
#4536 = DIRECTION ( 'NONE',  ( -0.9876526153536341335, -0.1566598588826327021, 0.000000000000000000 ) ) ;
#4538 = VECTOR ( 'NONE', #2201, 1000.000000000000000 ) ;
#4539 = VERTEX_POINT ( 'NONE', #17338 ) ;
#4540 = DIRECTION ( 'NONE',  ( -0.000000000000000000, -0.000000000000000000, -1.000000000000000000 ) ) ;
#4541 = CIRCLE ( 'NONE', #6672, 1.500000000000001332 ) ;
#4542 = EDGE_LOOP ( 'NONE', ( #11693, #8331, #12039, #7668 ) ) ;
#4543 = EDGE_LOOP ( 'NONE', ( #17886, #4014 ) ) ;
#4544 = DIRECTION ( 'NONE',  ( 2.735665993912342121E-16, 0.000000000000000000, 1.000000000000000000 ) ) ;
#4545 = DIRECTION ( 'NONE',  ( -0.1566598588826321192, 0.9876526153536342445, 7.798540720466730171E-17 ) ) ;
#4546 = CIRCLE ( 'NONE', #18532, 1.500000000000000000 ) ;
#4547 = DIRECTION ( 'NONE',  ( -0.9876526153536344665, -0.1566598588826304539, 0.000000000000000000 ) ) ;
#4548 = AXIS2_PLACEMENT_3D ( 'NONE', #2777, #13423, #15044 ) ;
#4549 = VERTEX_POINT ( 'NONE', #2978 ) ;
#4550 = EDGE_CURVE ( 'NONE', #5489, #12882, #2105, .T. ) ;
#4551 = AXIS2_PLACEMENT_3D ( 'NONE', #11371, #14616, #3044 ) ;
#4552 = ADVANCED_FACE ( 'NONE', ( #15109 ), #6320, .T. ) ;
#4553 = VECTOR ( 'NONE', #5561, 1000.000000000000000 ) ;
#4554 = CIRCLE ( 'NONE', #17811, 1.500000000000000888 ) ;
#4555 = ORIENTED_EDGE ( 'NONE', *, *, #1349, .F. ) ;
#4556 = FACE_BOUND ( 'NONE', #13903, .T. ) ;
#4557 = AXIS2_PLACEMENT_3D ( 'NONE', #13117, #3157, #11500 ) ;
#4558 = PLANE ( 'NONE',  #17659 ) ;
#4559 = EDGE_LOOP ( 'NONE', ( #6568, #5457 ) ) ;
#4560 = CARTESIAN_POINT ( 'NONE',  ( -54.73174206751432536, -23.86873732788596314, 4.330127018922218518 ) ) ;
#4561 = DIRECTION ( 'NONE',  ( 0.000000000000000000, 0.000000000000000000, -1.000000000000000000 ) ) ;
#4562 = TOROIDAL_SURFACE ( 'NONE', #5482, 3.000000000000004441, 2.000000000000000000 ) ;
#4563 = CARTESIAN_POINT ( 'NONE',  ( -68.72359699322777260, -88.85607972424169532, 8.660254037844412167 ) ) ;
#4564 = ORIENTED_EDGE ( 'NONE', *, *, #9378, .F. ) ;
#4565 = ORIENTED_EDGE ( 'NONE', *, *, #2752, .F. ) ;
#4566 = ORIENTED_EDGE ( 'NONE', *, *, #19, .F. ) ;
#4567 = CARTESIAN_POINT ( 'NONE',  ( -172.0951522251743029, 56.61964399677355431, -2.500000000000000000 ) ) ;
#4568 = FACE_BOUND ( 'NONE', #10941, .T. ) ;
#4569 = CARTESIAN_POINT ( 'NONE',  ( -43.04462899403342391, -84.78292339329327376, -21.65063509461098690 ) ) ;
#4570 = ORIENTED_EDGE ( 'NONE', *, *, #9491, .T. ) ;
#4571 = LINE ( 'NONE', #17590, #3039 ) ;
#4572 = EDGE_LOOP ( 'NONE', ( #6973, #5826, #13187, #15819 ) ) ;
#4573 = EDGE_CURVE ( 'NONE', #16485, #2390, #17902, .T. ) ;
#4574 = CIRCLE ( 'NONE', #5806, 2.000000000000001776 ) ;
#4575 = VERTEX_POINT ( 'NONE', #7644 ) ;
#4576 = DIRECTION ( 'NONE',  ( -0.1566598588826321192, 0.9876526153536342445, 7.798540720466730171E-17 ) ) ;
#4577 = VECTOR ( 'NONE', #6642, 1000.000000000000000 ) ;
#4578 = EDGE_CURVE ( 'NONE', #14627, #6069, #3007, .T. ) ;
#4579 = DIRECTION ( 'NONE',  ( -0.1566598588826321192, 0.9876526153536342445, 7.798540720466731404E-17 ) ) ;
#4580 = CARTESIAN_POINT ( 'NONE',  ( -61.15148406731293562, -24.88702641062306498, 4.330127018922218518 ) ) ;
#4581 = VECTOR ( 'NONE', #4191, 1000.000000000000000 ) ;
#4582 = CARTESIAN_POINT ( 'NONE',  ( -72.57555729771728181, 46.09591126511114112, -3.005167547231827996 ) ) ;
#4583 = DIRECTION ( 'NONE',  ( -0.9876526153536336894, -0.1566598588826349503, 0.000000000000000000 ) ) ;
#4584 = ORIENTED_EDGE ( 'NONE', *, *, #783, .F. ) ;
#4585 = ORIENTED_EDGE ( 'NONE', *, *, #2521, .T. ) ;
#4586 = FACE_BOUND ( 'NONE', #17262, .T. ) ;
#4587 = CARTESIAN_POINT ( 'NONE',  ( 0.000000000000000000, 0.000000000000000000, 25.00000000000000000 ) ) ;
#4588 = CARTESIAN_POINT ( 'NONE',  ( -6.995308533625909320, -79.06483854407720457, -21.65063509461098690 ) ) ;
#4589 = CIRCLE ( 'NONE', #14578, 1.499999999999999556 ) ;
#4590 = ORIENTED_EDGE ( 'NONE', *, *, #15913, .T. ) ;
#4591 = CARTESIAN_POINT ( 'NONE',  ( 10.28861223506262412, -76.32329101363113466, 17.32050807568880657 ) ) ;
#4592 = CARTESIAN_POINT ( 'NONE',  ( -3.382878129548365198, -13.70423786865299753, -130.3485206753969976 ) ) ;
#4593 = CIRCLE ( 'NONE', #13675, 12.74754878398197633 ) ;
#4594 = CIRCLE ( 'NONE', #5204, 1.500000000000000888 ) ;
#4595 = DIRECTION ( 'NONE',  ( -0.1566598588826321192, 0.9876526153536342445, 7.798540720466731404E-17 ) ) ;
#4596 = LINE ( 'NONE', #10281, #14847 ) ;
#4597 = DIRECTION ( 'NONE',  ( -0.1566598588826321192, 0.9876526153536342445, 7.798540720466730171E-17 ) ) ;
#4598 = AXIS2_PLACEMENT_3D ( 'NONE', #10700, #2750, #14216 ) ;
#4599 = ADVANCED_FACE ( 'NONE', ( #6130 ), #3436, .F. ) ;
#4600 = DIRECTION ( 'NONE',  ( -0.9876526153536336894, -0.1566598588826349503, 0.000000000000000000 ) ) ;
#4601 = CARTESIAN_POINT ( 'NONE',  ( -75.96627329761737712, -27.23692429386254332, 12.99038105676661736 ) ) ;
#4602 = EDGE_LOOP ( 'NONE', ( #494, #8655 ) ) ;
#4603 = DIRECTION ( 'NONE',  ( -0.1566598588826321192, 0.9876526153536342445, 7.798540720466730171E-17 ) ) ;
#4604 = ORIENTED_EDGE ( 'NONE', *, *, #6698, .F. ) ;
#4605 = FACE_BOUND ( 'NONE', #1972, .T. ) ;
#4606 = EDGE_LOOP ( 'NONE', ( #381, #3495, #1272, #6713 ) ) ;
#4607 = EDGE_CURVE ( 'NONE', #10635, #897, #9327, .T. ) ;
#4608 = EDGE_LOOP ( 'NONE', ( #9013, #429, #18050, #7987 ) ) ;
#4609 = EDGE_CURVE ( 'NONE', #14, #730, #282, .T. ) ;
#4610 = VERTEX_POINT ( 'NONE', #18079 ) ;
#4611 = VERTEX_POINT ( 'NONE', #5048 ) ;
#4612 = LINE ( 'NONE', #1869, #5971 ) ;
#4613 = CARTESIAN_POINT ( 'NONE',  ( -6.047290928450125946, -21.20899724884646531, 12.99038105676661026 ) ) ;
#4614 = CARTESIAN_POINT ( 'NONE',  ( -78.43540483600145308, -27.62857394106912423, 17.32050807568882078 ) ) ;
#4615 = CARTESIAN_POINT ( 'NONE',  ( -21.84973277410820458, -23.71555499096855613, 1.887572821959364500E-14 ) ) ;
#4616 = CARTESIAN_POINT ( 'NONE',  ( -6.007655918272284623, -78.90817868519457079, 8.660254037844408614 ) ) ;
#4617 = PRESENTATION_STYLE_ASSIGNMENT (( #1687 ) ) ;
#4618 = DIRECTION ( 'NONE',  ( -0.9876526153536336894, -0.1566598588826349503, 0.000000000000000000 ) ) ;
#4619 = LINE ( 'NONE', #14587, #5735 ) ;
#4620 = VERTEX_POINT ( 'NONE', #10821 ) ;
#4621 = DIRECTION ( 'NONE',  ( 0.000000000000000000, 0.000000000000000000, 1.000000000000000000 ) ) ;
#4622 = EDGE_CURVE ( 'NONE', #227, #11803, #5757, .T. ) ;
#4623 = CARTESIAN_POINT ( 'NONE',  ( 0.4120860815263194254, -77.88988960245745830, 8.660254037844408614 ) ) ;
#4624 = CARTESIAN_POINT ( 'NONE',  ( -14.93616446663280328, -22.61893597879013740, -17.32050807568878170 ) ) ;
#4625 = ORIENTED_EDGE ( 'NONE', *, *, #14894, .T. ) ;
#4626 = EDGE_CURVE ( 'NONE', #7186, #3590, #3622, .T. ) ;
#4628 = ORIENTED_EDGE ( 'NONE', *, *, #9298, .F. ) ;
#4627 = LINE ( 'NONE', #15046, #3589 ) ;
#4629 = EDGE_CURVE ( 'NONE', #10665, #15027, #9370, .T. ) ;
#4630 = EDGE_LOOP ( 'NONE', ( #6779, #2547, #9147, #4827 ) ) ;
#4631 = DIRECTION ( 'NONE',  ( -0.9876526153536341335, -0.1566598588826327021, 0.000000000000000000 ) ) ;
#4632 = AXIS2_PLACEMENT_3D ( 'NONE', #11061, #9472, #12493 ) ;
#4633 = EDGE_CURVE ( 'NONE', #8008, #15653, #6221, .T. ) ;
#4634 = ORIENTED_EDGE ( 'NONE', *, *, #4607, .F. ) ;
#4635 = ORIENTED_EDGE ( 'NONE', *, *, #11579, .T. ) ;
#4636 = ORIENTED_EDGE ( 'NONE', *, *, #8156, .F. ) ;
#4637 = DIRECTION ( 'NONE',  ( -0.9876526153536336894, -0.1566598588826350336, 0.000000000000000000 ) ) ;
#4638 = CARTESIAN_POINT ( 'NONE',  ( -44.07191661956488105, -27.24040181582776299, -4.330127018922181215 ) ) ;
#4639 = CYLINDRICAL_SURFACE ( 'NONE', #7371, 1.500000000000001554 ) ;
#4640 = AXIS2_PLACEMENT_3D ( 'NONE', #17725, #548, #10676 ) ;
#4641 = LINE ( 'NONE', #11909, #253 ) ;
#4642 = CARTESIAN_POINT ( 'NONE',  ( 0.000000000000000000, 0.000000000000000000, -30.00000000000000000 ) ) ;
#4643 = EDGE_LOOP ( 'NONE', ( #10514, #16463 ) ) ;
#4644 = EDGE_CURVE ( 'NONE', #8469, #5396, #16641, .T. ) ;
#4645 = ADVANCED_FACE ( 'NONE', ( #17033 ), #5258, .F. ) ;
#4646 = EDGE_LOOP ( 'NONE', ( #4355, #8636 ) ) ;
#4647 = CARTESIAN_POINT ( 'NONE',  ( -23.33121169713865584, -23.95054477929251036, -17.32050807568878170 ) ) ;
#4649 = EDGE_CURVE ( 'NONE', #9397, #7505, #18185, .T. ) ;
#4648 = DIRECTION ( 'NONE',  ( 0.000000000000000000, 0.000000000000000000, 1.000000000000000000 ) ) ;
#4650 = VERTEX_POINT ( 'NONE', #2221 ) ;
#4651 = EDGE_CURVE ( 'NONE', #8287, #14949, #1229, .T. ) ;
#4652 = EDGE_LOOP ( 'NONE', ( #12016, #11274, #8, #15733 ) ) ;
#4653 = ORIENTED_EDGE ( 'NONE', *, *, #15865, .T. ) ;
#4654 = FACE_OUTER_BOUND ( 'NONE', #4714, .T. ) ;
#4655 = FACE_BOUND ( 'NONE', #8658, .T. ) ;
#4656 = DIRECTION ( 'NONE',  ( -0.1566598588826321192, 0.9876526153536342445, 7.798540720466731404E-17 ) ) ;
#4657 = VERTEX_POINT ( 'NONE', #16746 ) ;
#4658 = DIRECTION ( 'NONE',  ( -0.9876526153536336894, -0.1566598588826349503, 0.000000000000000000 ) ) ;
#4659 = ORIENTED_EDGE ( 'NONE', *, *, #8346, .T. ) ;
#4660 = VERTEX_POINT ( 'NONE', #15290 ) ;
#4661 = ORIENTED_EDGE ( 'NONE', *, *, #3453, .F. ) ;
#4662 = DIRECTION ( 'NONE',  ( -0.1566598588826321192, 0.9876526153536342445, 7.798540720466731404E-17 ) ) ;
#4663 = DIRECTION ( 'NONE',  ( -0.1566598588826321192, 0.9876526153536342445, 7.798540720466730171E-17 ) ) ;
#4664 = DIRECTION ( 'NONE',  ( -0.9876526153536341335, -0.1566598588826327021, 0.000000000000000000 ) ) ;
#4665 = CARTESIAN_POINT ( 'NONE',  ( -66.29410046502155751, -30.76524864068697696, 17.32050807568881723 ) ) ;
#4666 = DIRECTION ( 'NONE',  ( -0.9876526153536336894, -0.1566598588826349503, 0.000000000000000000 ) ) ;
#4667 = ORIENTED_EDGE ( 'NONE', *, *, #10531, .T. ) ;
#4668 = CARTESIAN_POINT ( 'NONE',  ( -22.79775037928398618, -81.57139628619931671, 8.660254037844412167 ) ) ;
#4669 = AXIS2_PLACEMENT_3D ( 'NONE', #11417, #17146, #9833 ) ;
#4670 = CARTESIAN_POINT ( 'NONE',  ( -67.73594437787414790, -88.69941986535904732, -21.65063509461098690 ) ) ;
#4671 = EDGE_CURVE ( 'NONE', #10521, #1565, #12375, .T. ) ;
#4672 = DIRECTION ( 'NONE',  ( -0.9876526153536336894, -0.1566598588826349503, 0.000000000000000000 ) ) ;
#4673 = EDGE_CURVE ( 'NONE', #9895, #5011, #4214, .T. ) ;
#4674 = EDGE_LOOP ( 'NONE', ( #5819, #12508, #1748, #15482 ) ) ;
#4675 = ORIENTED_EDGE ( 'NONE', *, *, #16432, .F. ) ;
#4676 = DIRECTION ( 'NONE',  ( -0.9876526153536336894, -0.1566598588826349503, 0.000000000000000000 ) ) ;
#4677 = EDGE_CURVE ( 'NONE', #9448, #10913, #8198, .T. ) ;
#4678 = DIRECTION ( 'NONE',  ( 2.671473304378624222E-16, 0.000000000000000000, 1.000000000000000000 ) ) ;
#4679 = AXIS2_PLACEMENT_3D ( 'NONE', #10831, #3632, #638 ) ;
#4680 = DIRECTION ( 'NONE',  ( 0.000000000000000000, 0.000000000000000000, 1.000000000000000000 ) ) ;
#4681 = ORIENTED_EDGE ( 'NONE', *, *, #10044, .F. ) ;
#4682 = DIRECTION ( 'NONE',  ( 0.000000000000000000, 0.000000000000000000, 1.000000000000000000 ) ) ;
#4683 = DIRECTION ( 'NONE',  ( -0.9876526153536336894, -0.1566598588826350336, 0.000000000000000000 ) ) ;
#4684 = CARTESIAN_POINT ( 'NONE',  ( -25.80034323552273179, -24.34219442649909126, -12.99038105676658006 ) ) ;
#4685 = DIRECTION ( 'NONE',  ( -1.547359998875406858E-16, 4.084688078942370972E-17, -1.000000000000000000 ) ) ;
#4686 = ORIENTED_EDGE ( 'NONE', *, *, #6296, .T. ) ;
#4687 = ORIENTED_EDGE ( 'NONE', *, *, #15847, .T. ) ;
#4688 = DIRECTION ( 'NONE',  ( -0.1566598588826321747, 0.9876526153536343555, 0.000000000000000000 ) ) ;
#4689 = ORIENTED_EDGE ( 'NONE', *, *, #1191, .T. ) ;
#4690 = EDGE_LOOP ( 'NONE', ( #14029, #408, #5920, #8744 ) ) ;
#4691 = ORIENTED_EDGE ( 'NONE', *, *, #6028, .F. ) ;
#4692 = CARTESIAN_POINT ( 'NONE',  ( -45.55339554259532520, -27.47539160415171722, 4.330127018922217630 ) ) ;
#4693 = CIRCLE ( 'NONE', #17445, 1.500000000000000888 ) ;
#4694 = ORIENTED_EDGE ( 'NONE', *, *, #1223, .F. ) ;
#4695 = ADVANCED_FACE ( 'NONE', ( #11107 ), #12825, .F. ) ;
#4696 = DIRECTION ( 'NONE',  ( -0.1566598588826321192, 0.9876526153536342445, 7.798540720466730171E-17 ) ) ;
#4697 = CARTESIAN_POINT ( 'NONE',  ( -90.00000000000000000, -35.00000000000002132, 30.00000000000002842 ) ) ;
#4698 = CARTESIAN_POINT ( 'NONE',  ( -81.73462711737164454, 33.01666666666666572, -35.00000000000000000 ) ) ;
#4699 = VECTOR ( 'NONE', #6717, 1000.000000000000000 ) ;
#4700 = FACE_OUTER_BOUND ( 'NONE', #4466, .T. ) ;
#4701 = ORIENTED_EDGE ( 'NONE', *, *, #9726, .F. ) ;
#4702 = CARTESIAN_POINT ( 'NONE',  ( 0.000000000000000000, 0.000000000000000000, -19.99999999999999645 ) ) ;
#4703 =( NAMED_UNIT ( * ) SI_UNIT ( $, .STERADIAN. ) SOLID_ANGLE_UNIT ( ) );
#4704 = ADVANCED_FACE ( 'NONE', ( #2466 ), #2645, .F. ) ;
#4705 = LINE ( 'NONE', #15139, #2074 ) ;
#4706 = CIRCLE ( 'NONE', #15310, 1.499999999999999556 ) ;
#4707 = ORIENTED_EDGE ( 'NONE', *, *, #8121, .T. ) ;
#4708 = DIRECTION ( 'NONE',  ( -0.9876526153536336894, -0.1566598588826349503, 0.000000000000000000 ) ) ;
#4709 = FACE_BOUND ( 'NONE', #18685, .T. ) ;
#4710 = LINE ( 'NONE', #7478, #14762 ) ;
#4712 = ORIENTED_EDGE ( 'NONE', *, *, #12537, .T. ) ;
#4711 = DIRECTION ( 'NONE',  ( -0.1566598588826321192, 0.9876526153536342445, 7.798540720466730171E-17 ) ) ;
#4713 = ORIENTED_EDGE ( 'NONE', *, *, #1558, .T. ) ;
#4714 = EDGE_LOOP ( 'NONE', ( #11329, #6235, #15047, #17467 ) ) ;
#4715 = CARTESIAN_POINT ( 'NONE',  ( -38.92930022185625205, -21.36217958576385811, 17.32050807568882078 ) ) ;
#4716 = AXIS2_PLACEMENT_3D ( 'NONE', #4927, #13546, #1644 ) ;
#4717 = EDGE_LOOP ( 'NONE', ( #11922, #16464, #4169, #8212 ) ) ;
#4718 = VERTEX_POINT ( 'NONE', #7038 ) ;
#4719 = CARTESIAN_POINT ( 'NONE',  ( -32.67427653282027933, -83.13799487502562613, 8.660254037844412167 ) ) ;
#4720 = VECTOR ( 'NONE', #17520, 1000.000000000000114 ) ;
#4721 = CARTESIAN_POINT ( 'NONE',  ( -38.10636591726525069, -83.99962409888011905, 12.99038105676661203 ) ) ;
#4722 = EDGE_LOOP ( 'NONE', ( #13567, #12736, #6734, #8957 ) ) ;
#4723 = EDGE_CURVE ( 'NONE', #16662, #15554, #8642, .T. ) ;
#4724 = CARTESIAN_POINT ( 'NONE',  ( -76.88921716020503538, -2.445151130096096193, -7.406988961241581571 ) ) ;
#4725 = DIRECTION ( 'NONE',  ( -0.1566598588826321192, 0.9876526153536342445, 7.798540720466731404E-17 ) ) ;
#4726 = EDGE_CURVE ( 'NONE', #9991, #17961, #14416, .T. ) ;
#4727 = UNCERTAINTY_MEASURE_WITH_UNIT (LENGTH_MEASURE( 1.000000000000000082E-05 ), #6132, 'distance_accuracy_value', 'NONE');
#4728 = DIRECTION ( 'NONE',  ( -0.9876526153536344665, -0.1566598588826304539, 0.000000000000000000 ) ) ;
#4729 = DIRECTION ( 'NONE',  ( 3.039628882124824168E-17, 0.000000000000000000, -1.000000000000000000 ) ) ;
#4730 = LINE ( 'NONE', #17846, #887 ) ;
#4731 = DIRECTION ( 'NONE',  ( -0.1566598588826321747, 0.9876526153536343555, 0.000000000000000000 ) ) ;
#4732 = EDGE_LOOP ( 'NONE', ( #10994, #18364, #1318, #7024 ) ) ;
#4733 = ORIENTED_EDGE ( 'NONE', *, *, #8809, .F. ) ;
#4734 = CARTESIAN_POINT ( 'NONE',  ( -66.08974714408108753, -25.67032570503622324, 4.330127018922218518 ) ) ;
#4735 = AXIS2_PLACEMENT_3D ( 'NONE', #6701, #10931, #3907 ) ;
#4736 = AXIS2_PLACEMENT_3D ( 'NONE', #182, #7484, #7678 ) ;
#4737 = CARTESIAN_POINT ( 'NONE',  ( -46.33669483700848701, -22.53712852738358308, -12.99038105676658006 ) ) ;
#4738 = AXIS2_PLACEMENT_3D ( 'NONE', #14848, #3266, #13326 ) ;
#4739 = ORIENTED_EDGE ( 'NONE', *, *, #6850, .T. ) ;
#4740 = ORIENTED_EDGE ( 'NONE', *, *, #18528, .F. ) ;
#4741 = VERTEX_POINT ( 'NONE', #5985 ) ;
#4742 = DIRECTION ( 'NONE',  ( -0.1566598588826321192, 0.9876526153536342445, 7.798540720466730171E-17 ) ) ;
#4743 = AXIS2_PLACEMENT_3D ( 'NONE', #922, #14549, #15784 ) ;
#4744 = EDGE_CURVE ( 'NONE', #15183, #8278, #10570, .T. ) ;
#4745 = AXIS2_PLACEMENT_3D ( 'NONE', #9639, #2434, #544 ) ;
#4746 = ORIENTED_EDGE ( 'NONE', *, *, #127, .F. ) ;
#4747 = EDGE_LOOP ( 'NONE', ( #17109, #4783 ) ) ;
#4748 = FACE_BOUND ( 'NONE', #1438, .T. ) ;
#4749 = EDGE_CURVE ( 'NONE', #3169, #450, #4817, .T. ) ;
#4750 = EDGE_CURVE ( 'NONE', #3775, #1828, #16035, .T. ) ;
#4751 = ORIENTED_EDGE ( 'NONE', *, *, #17417, .F. ) ;
#4752 = ORIENTED_EDGE ( 'NONE', *, *, #1192, .F. ) ;
#4753 = VECTOR ( 'NONE', #9266, 1000.000000000000000 ) ;
#4754 = VERTEX_POINT ( 'NONE', #15846 ) ;
#4755 = CARTESIAN_POINT ( 'NONE',  ( -175.0529311237955881, 56.11526690008648899, -2.500000000000065725 ) ) ;
#4756 = FACE_BOUND ( 'NONE', #566, .T. ) ;
#4757 = VECTOR ( 'NONE', #330, 1000.000000000000000 ) ;
#4758 = FACE_OUTER_BOUND ( 'NONE', #8170, .T. ) ;
#4759 = DIRECTION ( 'NONE',  ( -1.000000000000000000, 0.000000000000000000, 0.000000000000000000 ) ) ;
#4760 = DIRECTION ( 'NONE',  ( -0.1566598588826321747, 0.9876526153536343555, 0.000000000000000000 ) ) ;
#4761 = CARTESIAN_POINT ( 'NONE',  ( -19.38060123572412863, -23.32390534376198232, -21.65063509461098334 ) ) ;
#4762 = CYLINDRICAL_SURFACE ( 'NONE', #12869, 1.500000000000001554 ) ;
#4763 = DIRECTION ( 'NONE',  ( -0.1566598588826321192, 0.9876526153536342445, 7.798540720466730171E-17 ) ) ;
#4764 = EDGE_LOOP ( 'NONE', ( #14428, #6762, #7513, #2011, #11123 ) ) ;
#4765 = ORIENTED_EDGE ( 'NONE', *, *, #13971, .T. ) ;
#4766 = CARTESIAN_POINT ( 'NONE',  ( 3.231158466157542541, -19.73726462726228803, 30.00000000000000000 ) ) ;
#4767 = DIRECTION ( 'NONE',  ( -0.1566598588826321192, 0.9876526153536342445, 7.798540720466730171E-17 ) ) ;
#4768 = DIRECTION ( 'NONE',  ( 0.1856185419698762329, -0.9826218788918640312, 0.000000000000000000 ) ) ;
#4769 = EDGE_LOOP ( 'NONE', ( #2821, #14933, #10668, #15763 ) ) ;
#4770 = ORIENTED_EDGE ( 'NONE', *, *, #16258, .T. ) ;
#4771 = CARTESIAN_POINT ( 'NONE',  ( -63.82496892663748156, -30.37359899348040315, 12.99038105676661736 ) ) ;
#4772 = CIRCLE ( 'NONE', #17821, 1.499999999999999556 ) ;
#4773 = FACE_BOUND ( 'NONE', #639, .T. ) ;
#4774 = CARTESIAN_POINT ( 'NONE',  ( -129.1404785418517918, -2.850701963179330445, 15.74754878398195856 ) ) ;
#4775 = CIRCLE ( 'NONE', #9638, 1.500000000000000888 ) ;
#4776 = DIRECTION ( 'NONE',  ( -0.9876526153536336894, -0.1566598588826349503, 0.000000000000000000 ) ) ;
#4777 = EDGE_CURVE ( 'NONE', #959, #2096, #17873, .T. ) ;
#4778 = ORIENTED_EDGE ( 'NONE', *, *, #7970, .T. ) ;
#4779 = ADVANCED_FACE ( 'NONE', ( #119 ), #14525, .F. ) ;
#4780 = DIRECTION ( 'NONE',  ( 1.000000000000000000, 0.000000000000000000, -0.000000000000000000 ) ) ;
#4781 = CYLINDRICAL_SURFACE ( 'NONE', #9585, 1.500000000000000666 ) ;
#4782 = FACE_OUTER_BOUND ( 'NONE', #16015, .T. ) ;
#4783 = ORIENTED_EDGE ( 'NONE', *, *, #5339, .F. ) ;
#4784 = ORIENTED_EDGE ( 'NONE', *, *, #12442, .F. ) ;
#4785 = CARTESIAN_POINT ( 'NONE',  ( -35.67686938905904270, -25.90879301532540779, -21.65063509461098334 ) ) ;
#4786 = ORIENTED_EDGE ( 'NONE', *, *, #6218, .T. ) ;
#4787 = AXIS2_PLACEMENT_3D ( 'NONE', #15207, #1020, #2222 ) ;
#4788 = ORIENTED_EDGE ( 'NONE', *, *, #10414, .T. ) ;
#4789 = ORIENTED_EDGE ( 'NONE', *, *, #14726, .F. ) ;
#4790 = DIRECTION ( 'NONE',  ( 0.000000000000000000, 0.000000000000000000, 1.000000000000000000 ) ) ;
#4791 = VECTOR ( 'NONE', #7597, 1000.000000000000000 ) ;
#4792 = DIRECTION ( 'NONE',  ( -0.1566598588826321192, 0.9876526153536342445, 7.798540720466730171E-17 ) ) ;
#4793 = DIRECTION ( 'NONE',  ( 0.000000000000000000, 0.000000000000000000, 1.000000000000000000 ) ) ;
#4794 = CIRCLE ( 'NONE', #15400, 1.500000000000000888 ) ;
#4795 = ORIENTED_EDGE ( 'NONE', *, *, #12887, .T. ) ;
#4796 = CARTESIAN_POINT ( 'NONE',  ( -17.85948730251583783, -80.78809699178614778, -17.32050807568878525 ) ) ;
#4797 = DIRECTION ( 'NONE',  ( -0.9826218788918642533, -0.1856185419698762884, 0.000000000000000000 ) ) ;
#4798 = CARTESIAN_POINT ( 'NONE',  ( 2.000000000000000000, 2.449293598294706414E-16, -35.00000000000000000 ) ) ;
#4799 = AXIS2_PLACEMENT_3D ( 'NONE', #5388, #12276, #2165 ) ;
#4800 = FACE_OUTER_BOUND ( 'NONE', #8513, .T. ) ;
#4801 = DIRECTION ( 'NONE',  ( -0.1566598588826321192, 0.9876526153536342445, 7.798540720466730171E-17 ) ) ;
#4802 = DIRECTION ( 'NONE',  ( 0.000000000000000000, 0.000000000000000000, 1.000000000000000000 ) ) ;
#4803 = ADVANCED_FACE ( 'NONE', ( #11642 ), #12064, .T. ) ;
#4804 = CARTESIAN_POINT ( 'NONE',  ( 7.819480696678551723, -76.71494066083772623, 4.330127018922207860 ) ) ;
#4806 = ORIENTED_EDGE ( 'NONE', *, *, #601, .F. ) ;
#4805 = CYLINDRICAL_SURFACE ( 'NONE', #1502, 1.500000000000001554 ) ;
#4807 = AXIS2_PLACEMENT_3D ( 'NONE', #13274, #10435, #3223 ) ;
#4808 = DIRECTION ( 'NONE',  ( -0.1566598588826321747, 0.9876526153536343555, 0.000000000000000000 ) ) ;
#4809 = AXIS2_PLACEMENT_3D ( 'NONE', #5803, #11540, #4358 ) ;
#4810 = VERTEX_POINT ( 'NONE', #17472 ) ;
#4811 = ADVANCED_FACE ( 'NONE', ( #12811 ), #8650, .F. ) ;
#4812 = ORIENTED_EDGE ( 'NONE', *, *, #2086, .T. ) ;
#4813 = CARTESIAN_POINT ( 'NONE',  ( -34.15575545585073058, -83.37298466334958391, 8.660254037844412167 ) ) ;
#4814 = AXIS2_PLACEMENT_3D ( 'NONE', #2619, #2444, #8229 ) ;
#4815 = AXIS2_PLACEMENT_3D ( 'NONE', #10460, #14832, #13479 ) ;
#4816 = AXIS2_PLACEMENT_3D ( 'NONE', #13681, #7479, #12344 ) ;
#4817 = CIRCLE ( 'NONE', #15124, 1.500000000000000444 ) ;
#4818 = LINE ( 'NONE', #17564, #9449 ) ;
#4819 = EDGE_LOOP ( 'NONE', ( #714, #9485 ) ) ;
#4820 = CARTESIAN_POINT ( 'NONE',  ( -52.26261052913027072, -23.47708768067937868, -8.660254037844380193 ) ) ;
#4821 = DIRECTION ( 'NONE',  ( 0.000000000000000000, 0.000000000000000000, 1.000000000000000000 ) ) ;
#4822 = DIRECTION ( 'NONE',  ( 1.000000000000000000, 0.000000000000000000, 0.000000000000000000 ) ) ;
#4823 = DIRECTION ( 'NONE',  ( 0.000000000000000000, 0.000000000000000000, 1.000000000000000000 ) ) ;
#4824 = CIRCLE ( 'NONE', #16980, 1.500000000000000888 ) ;
#4825 = DIRECTION ( 'NONE',  ( -0.9876526153536341335, -0.1566598588826327021, 0.000000000000000000 ) ) ;
#4826 = DIRECTION ( 'NONE',  ( -0.1566598588826321192, 0.9876526153536342445, 7.798540720466731404E-17 ) ) ;
#4827 = ORIENTED_EDGE ( 'NONE', *, *, #3079, .T. ) ;
#4828 = CIRCLE ( 'NONE', #2718, 1.500000000000000444 ) ;
#4829 = CARTESIAN_POINT ( 'NONE',  ( -20.86208015875458344, -23.55889513208593655, 21.65063509461101177 ) ) ;
#4830 = VERTEX_POINT ( 'NONE', #4181 ) ;
#4831 = ADVANCED_FACE ( 'NONE', ( #1365 ), #9965, .F. ) ;
#4832 = CARTESIAN_POINT ( 'NONE',  ( -52.96079015774756016, -28.65034054577145994, 1.869203119972154228E-14 ) ) ;
#4833 = CARTESIAN_POINT ( 'NONE',  ( -172.0951522251743029, 56.61964399677356141, 2.500000000000000000 ) ) ;
#4834 = ORIENTED_EDGE ( 'NONE', *, *, #17615, .F. ) ;
#4835 = ADVANCED_FACE ( 'NONE', ( #30 ), #4460, .F. ) ;
#4836 = VERTEX_POINT ( 'NONE', #8835 ) ;
#4837 = AXIS2_PLACEMENT_3D ( 'NONE', #9345, #6810, #1042 ) ;
#4838 = ORIENTED_EDGE ( 'NONE', *, *, #14687, .T. ) ;
#4839 = DIRECTION ( 'NONE',  ( -0.9876526153536336894, -0.1566598588826349503, 0.000000000000000000 ) ) ;
#4840 = ORIENTED_EDGE ( 'NONE', *, *, #3895, .F. ) ;
#4841 = CIRCLE ( 'NONE', #17293, 1.499999999999999556 ) ;
#4842 = FACE_BOUND ( 'NONE', #13068, .T. ) ;
#4843 = VECTOR ( 'NONE', #11753, 1000.000000000000000 ) ;
#4844 = EDGE_LOOP ( 'NONE', ( #15254, #1407 ) ) ;
#4845 = CARTESIAN_POINT ( 'NONE',  ( -76.90911978745816668, 1.387778780781445676E-14, 25.00000000000000000 ) ) ;
#4846 = AXIS2_PLACEMENT_3D ( 'NONE', #6368, #2177, #15058 ) ;
#4847 = EDGE_LOOP ( 'NONE', ( #11935, #177, #16663, #3020 ) ) ;
#4848 = EDGE_LOOP ( 'NONE', ( #6680, #3325 ) ) ;
#4849 = EDGE_CURVE ( 'NONE', #1556, #3175, #7849, .T. ) ;
#4850 = AXIS2_PLACEMENT_3D ( 'NONE', #3801, #12049, #16534 ) ;
#4851 = CARTESIAN_POINT ( 'NONE',  ( -88.14047854185180597, 6.938893903907228378E-15, 30.00000000000000000 ) ) ;
#4853 = DIRECTION ( 'NONE',  ( -0.9876526153536341335, -0.1566598588826327021, 0.000000000000000000 ) ) ;
#4852 = CIRCLE ( 'NONE', #7898, 5.000000000000000000 ) ;
#4854 = CARTESIAN_POINT ( 'NONE',  ( -5.349111299832828514, -16.03574438375436984, 4.330127018922214965 ) ) ;
#4855 = LINE ( 'NONE', #11860, #2277 ) ;
#4856 = ADVANCED_FACE ( 'NONE', ( #3046, #7415 ), #13170, .F. ) ;
#4857 = DIRECTION ( 'NONE',  ( 1.000000000000000000, -0.000000000000000000, -0.000000000000000000 ) ) ;
#4858 = ORIENTED_EDGE ( 'NONE', *, *, #17861, .F. ) ;
#4859 = ORIENTED_EDGE ( 'NONE', *, *, #960, .F. ) ;
#4860 = DIRECTION ( 'NONE',  ( 0.000000000000000000, 0.000000000000000000, -1.000000000000000000 ) ) ;
#4861 = EDGE_CURVE ( 'NONE', #1457, #1168, #2942, .T. ) ;
#4862 = EDGE_CURVE ( 'NONE', #491, #15907, #5736, .T. ) ;
#4863 = CARTESIAN_POINT ( 'NONE',  ( -129.1404785418517918, 9.649298036820672664, -2.500000000000007994 ) ) ;
#4864 = CIRCLE ( 'NONE', #14259, 2.200000000000000622 ) ;
#4865 = EDGE_LOOP ( 'NONE', ( #15914, #16088 ) ) ;
#4866 = DIRECTION ( 'NONE',  ( -0.1566598588826321192, 0.9876526153536342445, 7.798540720466730171E-17 ) ) ;
#4867 = EDGE_CURVE ( 'NONE', #18009, #9527, #5603, .T. ) ;
#4868 = CIRCLE ( 'NONE', #1566, 12.83663829214476948 ) ;
#4869 = EDGE_LOOP ( 'NONE', ( #3151, #7094 ) ) ;
#4870 = CARTESIAN_POINT ( 'NONE',  ( -49.26481467677529480, 51.83848025225069733, 20.00000000000001421 ) ) ;
#4871 = VECTOR ( 'NONE', #715, 1000.000000000000000 ) ;
#4872 = DIRECTION ( 'NONE',  ( -1.000000000000000000, 0.000000000000000000, 0.000000000000000000 ) ) ;
#4873 = CARTESIAN_POINT ( 'NONE',  ( -50.49165861936347000, -28.25869089856487903, 21.65063509461101887 ) ) ;
#4874 = CIRCLE ( 'NONE', #974, 1.500000000000000444 ) ;
#4875 = DIRECTION ( 'NONE',  ( -1.000000000000000000, 0.000000000000000000, 0.000000000000000000 ) ) ;
#4876 = DIRECTION ( 'NONE',  ( -0.1566598588826321192, 0.9876526153536342445, 7.798540720466731404E-17 ) ) ;
#4877 = AXIS2_PLACEMENT_3D ( 'NONE', #17266, #11523, #7209 ) ;
#4878 = AXIS2_PLACEMENT_3D ( 'NONE', #15267, #5328, #6956 ) ;
#4879 = DIRECTION ( 'NONE',  ( -0.1566598588826321192, 0.9876526153536342445, 7.798540720466730171E-17 ) ) ;
#4880 = EDGE_CURVE ( 'NONE', #584, #18389, #7398, .T. ) ;
#4881 = ORIENTED_EDGE ( 'NONE', *, *, #17949, .F. ) ;
#4882 = EDGE_LOOP ( 'NONE', ( #9630, #5173, #15590, #4420 ) ) ;
#4883 = DIRECTION ( 'NONE',  ( -0.1566598588826321192, 0.9876526153536342445, 7.798540720466730171E-17 ) ) ;
#4884 = EDGE_LOOP ( 'NONE', ( #9777, #6067, #17131, #820 ) ) ;
#4885 = ORIENTED_EDGE ( 'NONE', *, *, #13124, .F. ) ;
#4886 = EDGE_CURVE ( 'NONE', #10150, #9162, #12048, .T. ) ;
#4887 = ORIENTED_EDGE ( 'NONE', *, *, #5076, .T. ) ;
#4888 = EDGE_CURVE ( 'NONE', #10626, #1132, #9354, .T. ) ;
#4889 = AXIS2_PLACEMENT_3D ( 'NONE', #16205, #3294, #1894 ) ;
#4890 = DIRECTION ( 'NONE',  ( -0.9876526153536341335, -0.1566598588826327576, 0.000000000000000000 ) ) ;
#4891 = MECHANICAL_DESIGN_GEOMETRIC_PRESENTATION_REPRESENTATION (  '', ( #7057 ), #11847 ) ;
#4892 = CYLINDRICAL_SURFACE ( 'NONE', #16708, 1.500000000000001554 ) ;
#4893 = CARTESIAN_POINT ( 'NONE',  ( -41.39843176024032800, -21.75382923297043547, 12.99038105676661736 ) ) ;
#4894 = LINE ( 'NONE', #10678, #9444 ) ;
#4895 = CYLINDRICAL_SURFACE ( 'NONE', #6005, 1.500000000000001554 ) ;
#4896 = FACE_OUTER_BOUND ( 'NONE', #1036, .T. ) ;
#4897 = CYLINDRICAL_SURFACE ( 'NONE', #15022, 1.500000000000001554 ) ;
#4898 = DIRECTION ( 'NONE',  ( 0.000000000000000000, 0.000000000000000000, 1.000000000000000000 ) ) ;
#4899 = ORIENTED_EDGE ( 'NONE', *, *, #5885, .F. ) ;
#4900 = DIRECTION ( 'NONE',  ( -0.1566598588826321192, 0.9876526153536342445, 7.798540720466730171E-17 ) ) ;
#4901 = DIRECTION ( 'NONE',  ( -0.9876526153536336894, -0.1566598588826350336, 0.000000000000000000 ) ) ;
#4903 = ORIENTED_EDGE ( 'NONE', *, *, #3125, .T. ) ;
#4902 = CARTESIAN_POINT ( 'NONE',  ( -14.23798483801550674, -17.44568311369805969, 1.908195823574487804E-14 ) ) ;
#4904 = CARTESIAN_POINT ( 'NONE',  ( 0.4120860815263194254, -77.88988960245745830, 8.660254037844408614 ) ) ;
#4905 = ORIENTED_EDGE ( 'NONE', *, *, #4241, .F. ) ;
#4906 = EDGE_CURVE ( 'NONE', #14051, #3263, #892, .T. ) ;
#4907 = ORIENTED_EDGE ( 'NONE', *, *, #6638, .T. ) ;
#4908 = CIRCLE ( 'NONE', #8562, 1.500000000000000888 ) ;
#4909 = EDGE_CURVE ( 'NONE', #16874, #9493, #8145, .T. ) ;
#4910 = CYLINDRICAL_SURFACE ( 'NONE', #15192, 1.500000000000001554 ) ;
#4911 = ORIENTED_EDGE ( 'NONE', *, *, #1108, .F. ) ;
#4912 = EDGE_CURVE ( 'NONE', #15608, #6427, #2383, .T. ) ;
#4913 = DIRECTION ( 'NONE',  ( -0.9876526153536336894, -0.1566598588826349503, 0.000000000000000000 ) ) ;
#4914 = CARTESIAN_POINT ( 'NONE',  ( 0.000000000000000000, 0.000000000000000000, 30.00000000000000000 ) ) ;
#4915 = UNCERTAINTY_MEASURE_WITH_UNIT (LENGTH_MEASURE( 1.000000000000000082E-05 ), #1474, 'distance_accuracy_value', 'NONE');
#4916 = CARTESIAN_POINT ( 'NONE',  ( -62.83731631128386397, -30.21693913459777647, -8.660254037844380193 ) ) ;
#4917 = CARTESIAN_POINT ( 'NONE',  ( -40.61513246582717329, -26.69209230973856251, -4.330127018922181215 ) ) ;
#4918 = CYLINDRICAL_SURFACE ( 'NONE', #7233, 1.500000000000001554 ) ;
#4919 = ORIENTED_EDGE ( 'NONE', *, *, #444, .T. ) ;
#4920 = DIRECTION ( 'NONE',  ( 1.000000000000000000, 0.000000000000000000, 0.000000000000000000 ) ) ;
#4921 = CIRCLE ( 'NONE', #16146, 1.500000000000001332 ) ;
#4922 = LINE ( 'NONE', #14978, #4383 ) ;
#4923 = FACE_OUTER_BOUND ( 'NONE', #469, .T. ) ;
#4924 = ORIENTED_EDGE ( 'NONE', *, *, #8809, .T. ) ;
#4925 = EDGE_LOOP ( 'NONE', ( #4334, #12632, #10246, #2343 ) ) ;
#4926 = VERTEX_POINT ( 'NONE', #7481 ) ;
#4927 = CARTESIAN_POINT ( 'NONE',  ( -51.43967622453926936, -86.11453219379563961, -4.330127018922185655 ) ) ;
#4928 = FACE_BOUND ( 'NONE', #17182, .T. ) ;
#4929 = VECTOR ( 'NONE', #9928, 1000.000000000000000 ) ;
#4930 = EDGE_CURVE ( 'NONE', #12097, #16672, #15406, .T. ) ;
#4931 = DIRECTION ( 'NONE',  ( -0.9876526153536336894, -0.1566598588826349503, 0.000000000000000000 ) ) ;
#4932 = CARTESIAN_POINT ( 'NONE',  ( -75.18297400320422241, -32.17518737063066681, -4.330127018922181215 ) ) ;
#4933 = EDGE_CURVE ( 'NONE', #10907, #8900, #13346, .T. ) ;
#4934 = FACE_OUTER_BOUND ( 'NONE', #6975, .T. ) ;
#4935 = CARTESIAN_POINT ( 'NONE',  ( -64.77298653181324539, -88.22944028871116018, -4.330127018922185655 ) ) ;
#4936 = DIRECTION ( 'NONE',  ( -1.000000000000000000, 0.000000000000000000, 0.000000000000000000 ) ) ;
#4937 = CARTESIAN_POINT ( 'NONE',  ( -84.16561914167408531, 33.59999999999999432, 30.00000000000000000 ) ) ;
#4938 = ORIENTED_EDGE ( 'NONE', *, *, #1494, .T. ) ;
#4939 = EDGE_LOOP ( 'NONE', ( #17204, #16241 ) ) ;
#4940 = DIRECTION ( 'NONE',  ( -0.9876526153536341335, -0.1566598588826327021, 0.000000000000000000 ) ) ;
#4941 = CARTESIAN_POINT ( 'NONE',  ( 73.09088021254186174, 1.387778780781445676E-14, -19.99999999999999645 ) ) ;
#4942 = ORIENTED_EDGE ( 'NONE', *, *, #8587, .T. ) ;
#4943 = ORIENTED_EDGE ( 'NONE', *, *, #8216, .F. ) ;
#4944 = DIRECTION ( 'NONE',  ( 0.000000000000000000, 0.000000000000000000, 1.000000000000000000 ) ) ;
#4945 = CARTESIAN_POINT ( 'NONE',  ( -32.67427653282027933, -83.13799487502562613, 1.443110928631665584E-14 ) ) ;
#4946 = DIRECTION ( 'NONE',  ( -0.1566598588826321192, 0.9876526153536342445, 7.798540720466730171E-17 ) ) ;
#4947 = ORIENTED_EDGE ( 'NONE', *, *, #7098, .T. ) ;
#4948 = EDGE_CURVE ( 'NONE', #6209, #16318, #3108, .T. ) ;
#4949 = DIRECTION ( 'NONE',  ( -0.9876526153536336894, -0.1566598588826349503, 0.000000000000000000 ) ) ;
#4950 = EDGE_CURVE ( 'NONE', #1906, #10635, #6165, .T. ) ;
#4951 = DIRECTION ( 'NONE',  ( -0.1566598588826321747, 0.9876526153536343555, 0.000000000000000000 ) ) ;
#4952 = CARTESIAN_POINT ( 'NONE',  ( 0.000000000000000000, 0.000000000000000000, 0.000000000000000000 ) ) ;
#4953 = ADVANCED_FACE ( 'NONE', ( #6355 ), #7676, .F. ) ;
#4954 = ORIENTED_EDGE ( 'NONE', *, *, #3581, .T. ) ;
#4955 = PLANE ( 'NONE',  #5770 ) ;
#4956 = DIRECTION ( 'NONE',  ( -0.9876526153536341335, -0.1566598588826327021, 0.000000000000000000 ) ) ;
#4957 = CARTESIAN_POINT ( 'NONE',  ( -68.55887868246516348, -26.06197535224279704, -8.660254037844380193 ) ) ;
#4958 = DIRECTION ( 'NONE',  ( 2.671473304378624222E-16, 0.000000000000000000, 1.000000000000000000 ) ) ;
#4959 = ORIENTED_EDGE ( 'NONE', *, *, #15456, .T. ) ;
#4960 = VERTEX_POINT ( 'NONE', #7754 ) ;
#4961 = CYLINDRICAL_SURFACE ( 'NONE', #15159, 1.500000000000001554 ) ;
#4962 = ORIENTED_EDGE ( 'NONE', *, *, #6335, .T. ) ;
#4963 = CARTESIAN_POINT ( 'NONE',  ( 11.77009115809307715, -76.08830122530719109, 17.32050807568880657 ) ) ;
#4964 = ORIENTED_EDGE ( 'NONE', *, *, #1647, .T. ) ;
#4965 = EDGE_CURVE ( 'NONE', #9953, #2455, #11452, .T. ) ;
#4966 = CIRCLE ( 'NONE', #7423, 2.000000000000000000 ) ;
#4967 = DIRECTION ( 'NONE',  ( -0.9876526153536341335, -0.1566598588826327576, 0.000000000000000000 ) ) ;
#4968 = EDGE_CURVE ( 'NONE', #62, #3665, #1696, .T. ) ;
#4969 = EDGE_CURVE ( 'NONE', #2351, #3651, #4627, .T. ) ;
#4970 = DIRECTION ( 'NONE',  ( -0.1566598588826321192, 0.9876526153536342445, 7.798540720466731404E-17 ) ) ;
#4971 = CARTESIAN_POINT ( 'NONE',  ( -5.349111299832828514, -16.03574438375436984, 12.99038105676661026 ) ) ;
#4972 = DIRECTION ( 'NONE',  ( -0.9876526153536336894, -0.1566598588826349503, 0.000000000000000000 ) ) ;
#4973 = FACE_OUTER_BOUND ( 'NONE', #9022, .T. ) ;
#4974 = PRODUCT_DEFINITION_SHAPE ( 'NONE', 'NONE',  #18797 ) ;
#4975 = LINE ( 'NONE', #2159, #14190 ) ;
#4976 = FACE_OUTER_BOUND ( 'NONE', #12617, .T. ) ;
#4977 = DIRECTION ( 'NONE',  ( -0.1566598588826321192, 0.9876526153536342445, 7.798540720466731404E-17 ) ) ;
#4978 = VERTEX_POINT ( 'NONE', #10400 ) ;
#4979 = LINE ( 'NONE', #14952, #10594 ) ;
#4980 = AXIS2_PLACEMENT_3D ( 'NONE', #9810, #2314, #15579 ) ;
#4982 = EDGE_LOOP ( 'NONE', ( #7342, #3670 ) ) ;
#4981 = CARTESIAN_POINT ( 'NONE',  ( 1.360103686702108128, -20.03404830722672259, 8.660254037844412167 ) ) ;
#4983 = CARTESIAN_POINT ( 'NONE',  ( -19.17624791478365864, -18.22898240811121440, -8.660254037844380193 ) ) ;
#4984 = EDGE_LOOP ( 'NONE', ( #11825, #15237, #1387, #11714 ) ) ;
#4985 = ORIENTED_EDGE ( 'NONE', *, *, #17809, .T. ) ;
#4986 = EDGE_LOOP ( 'NONE', ( #7336, #619, #17971, #18122, #2397, #3995 ) ) ;
#4987 = DIRECTION ( 'NONE',  ( -0.9876526153536341335, -0.1566598588826327021, 0.000000000000000000 ) ) ;
#4988 = EDGE_LOOP ( 'NONE', ( #54, #14843 ) ) ;
#4989 = DIRECTION ( 'NONE',  ( -0.9876526153536341335, -0.1566598588826327021, 0.000000000000000000 ) ) ;
#4990 = AXIS2_PLACEMENT_3D ( 'NONE', #16732, #2386, #9504 ) ;
#4991 = ORIENTED_EDGE ( 'NONE', *, *, #4607, .T. ) ;
#4992 = DIRECTION ( 'NONE',  ( -0.1566598588826321192, 0.9876526153536342445, 7.798540720466730171E-17 ) ) ;
#4993 = CYLINDRICAL_SURFACE ( 'NONE', #12746, 1.500000000000001554 ) ;
#4994 = DIRECTION ( 'NONE',  ( -0.9876526153536341335, -0.1566598588826327021, 0.000000000000000000 ) ) ;
#4995 = DIRECTION ( 'NONE',  ( -0.9876526153536336894, -0.1566598588826349503, 0.000000000000000000 ) ) ;
#4996 = VERTEX_POINT ( 'NONE', #1786 ) ;
#4997 = CARTESIAN_POINT ( 'NONE',  ( -10.98555400521827963, -21.99229654325962002, -4.330127018922181215 ) ) ;
#4998 = VERTEX_POINT ( 'NONE', #11896 ) ;
#4999 = ADVANCED_FACE ( 'NONE', ( #465 ), #4805, .F. ) ;
#5000 = ADVANCED_FACE ( 'NONE', ( #10491 ), #16285, .F. ) ;
#5001 = CARTESIAN_POINT ( 'NONE',  ( -71.72618984946653597, -31.62687786454144856, 21.65063509461101887 ) ) ;
#5002 = DIRECTION ( 'NONE',  ( -0.000000000000000000, -0.000000000000000000, -1.000000000000000000 ) ) ;
#5003 = AXIS2_PLACEMENT_3D ( 'NONE', #16912, #13943, #2576 ) ;
#5004 = DIRECTION ( 'NONE',  ( -0.9876526153536341335, -0.1566598588826327576, 0.000000000000000000 ) ) ;
#5005 = VERTEX_POINT ( 'NONE', #3376 ) ;
#5006 = FACE_BOUND ( 'NONE', #6253, .T. ) ;
#5007 = ADVANCED_FACE ( 'NONE', ( #1884 ), #6066, .T. ) ;
#5008 = AXIS2_PLACEMENT_3D ( 'NONE', #3014, #8626, #5878 ) ;
#5009 = ORIENTED_EDGE ( 'NONE', *, *, #4374, .F. ) ;
#5010 = EDGE_LOOP ( 'NONE', ( #5235, #13979, #10166, #10428 ) ) ;
#5011 = VERTEX_POINT ( 'NONE', #664 ) ;
#5012 = ORIENTED_EDGE ( 'NONE', *, *, #10660, .T. ) ;
#5013 = CARTESIAN_POINT ( 'NONE',  ( -26.78799585087635649, -24.49885428538171794, 8.660254037844417496 ) ) ;
#5014 = ORIENTED_EDGE ( 'NONE', *, *, #7525, .F. ) ;
#5015 = FACE_BOUND ( 'NONE', #18674, .T. ) ;
#5016 = ORIENTED_EDGE ( 'NONE', *, *, #3125, .F. ) ;
#5017 = CARTESIAN_POINT ( 'NONE',  ( -36.46016868347218320, -20.97052993855727365, 4.330127018922218518 ) ) ;
#5018 = SURFACE_SIDE_STYLE ('',( #10633 ) ) ;
#5019 = AXIS2_PLACEMENT_3D ( 'NONE', #4505, #73, #17344 ) ;
#5020 = FACE_BOUND ( 'NONE', #511, .T. ) ;
#5021 = CARTESIAN_POINT ( 'NONE',  ( -16.87183468716221313, -80.63143713290352821, -21.65063509461098690 ) ) ;
#5022 = ORIENTED_EDGE ( 'NONE', *, *, #13522, .F. ) ;
#5023 = CARTESIAN_POINT ( 'NONE',  ( 6.831828081324923474, -76.87160051972034580, 17.32050807568880657 ) ) ;
#5024 = CARTESIAN_POINT ( 'NONE',  ( 5.000000000000000000, 0.000000000000000000, 35.00000000000000000 ) ) ;
#5025 = CIRCLE ( 'NONE', #4131, 13.99999999999999822 ) ;
#5026 = ORIENTED_EDGE ( 'NONE', *, *, #11038, .F. ) ;
#5027 = CARTESIAN_POINT ( 'NONE',  ( -73.49714175923330117, -26.84527464665595531, -8.660254037844380193 ) ) ;
#5028 = CIRCLE ( 'NONE', #10773, 12.74754878398197633 ) ;
#5029 = ADVANCED_FACE ( 'NONE', ( #13514 ), #13425, .F. ) ;
#5030 = CARTESIAN_POINT ( 'NONE',  ( -66.78792677269838407, -30.84357857012830095, -12.99038105676658006 ) ) ;
#5031 = ORIENTED_EDGE ( 'NONE', *, *, #1119, .T. ) ;
#5032 = CARTESIAN_POINT ( 'NONE',  ( -14.40270314877813895, -80.23978748569695085, 1.424741226644455312E-14 ) ) ;
#5033 = CARTESIAN_POINT ( 'NONE',  ( 0.3724510713484785462, -20.19070816610934926, -21.65063509461098334 ) ) ;
#5034 = EDGE_LOOP ( 'NONE', ( #6830, #5867, #11121, #17385 ) ) ;
#5035 = DIRECTION ( 'NONE',  ( 0.000000000000000000, 0.000000000000000000, 1.000000000000000000 ) ) ;
#5036 = ORIENTED_EDGE ( 'NONE', *, *, #362, .T. ) ;
#5037 = PRESENTATION_LAYER_ASSIGNMENT (  '', '', ( #13213 ) ) ;
#5038 = ORIENTED_EDGE ( 'NONE', *, *, #653, .F. ) ;
#5039 = FACE_OUTER_BOUND ( 'NONE', #12305, .T. ) ;
#5040 = EDGE_CURVE ( 'NONE', #18006, #3093, #1782, .T. ) ;
#5041 = AXIS2_PLACEMENT_3D ( 'NONE', #7584, #13072, #16399 ) ;
#5042 = DIRECTION ( 'NONE',  ( -0.1566598588826321192, 0.9876526153536342445, 7.798540720466730171E-17 ) ) ;
#5043 = EDGE_LOOP ( 'NONE', ( #6788, #14911 ) ) ;
#5044 = EDGE_CURVE ( 'NONE', #17089, #9050, #11146, .T. ) ;
#5045 = FACE_BOUND ( 'NONE', #4819, .T. ) ;
#5046 = CIRCLE ( 'NONE', #7492, 1.500000000000001332 ) ;
#5047 = CARTESIAN_POINT ( 'NONE',  ( -30.73860631229088369, -25.12549372091224598, 4.330127018922217630 ) ) ;
#5048 = CARTESIAN_POINT ( 'NONE',  ( -79.24244631363546887, 32.81909429640987952, -30.00000000000000000 ) ) ;
#5049 = DIRECTION ( 'NONE',  ( -0.1566598588826321192, 0.9876526153536342445, 7.798540720466730171E-17 ) ) ;
#5050 = DIRECTION ( 'NONE',  ( 1.000000000000000000, 0.000000000000000000, 0.000000000000000000 ) ) ;
#5051 = CARTESIAN_POINT ( 'NONE',  ( -18.18859529943003750, -18.07232254922858417, 21.65063509461101177 ) ) ;
#5052 = DIRECTION ( 'NONE',  ( -0.1566598588826321192, 0.9876526153536342445, 7.798540720466730171E-17 ) ) ;
#5053 = AXIS2_PLACEMENT_3D ( 'NONE', #11013, #5260, #12245 ) ;
#5054 = CIRCLE ( 'NONE', #17804, 2.000000000000000000 ) ;
#5055 = CARTESIAN_POINT ( 'NONE',  ( -64.20000000000000284, 2.694222958124175527E-16, 25.00000000000000000 ) ) ;
#5056 = CARTESIAN_POINT ( 'NONE',  ( -38.10636591726527911, -83.99962409888010484, -21.65063509461098690 ) ) ;
#5057 = CARTESIAN_POINT ( 'NONE',  ( -15.92381708198643153, -22.77559583767277473, 21.65063509461101177 ) ) ;
#5058 = ORIENTED_EDGE ( 'NONE', *, *, #7707, .T. ) ;
#5059 = VERTEX_POINT ( 'NONE', #5292 ) ;
#5060 = DIRECTION ( 'NONE',  ( 1.000000000000000000, 0.000000000000000000, 0.000000000000000000 ) ) ;
#5061 = EDGE_CURVE ( 'NONE', #9479, #18003, #3841, .T. ) ;
#5062 = ORIENTED_EDGE ( 'NONE', *, *, #6970, .F. ) ;
#5063 = ORIENTED_EDGE ( 'NONE', *, *, #7474, .F. ) ;
#5064 = ORIENTED_EDGE ( 'NONE', *, *, #13666, .T. ) ;
#5065 = ADVANCED_FACE ( 'NONE', ( #1056 ), #18421, .F. ) ;
#5066 = CYLINDRICAL_SURFACE ( 'NONE', #6022, 1.500000000000001554 ) ;
#5067 = CYLINDRICAL_SURFACE ( 'NONE', #12906, 1.500000000000001554 ) ;
#5068 = AXIS2_PLACEMENT_3D ( 'NONE', #3304, #13638, #10513 ) ;
#5069 = ORIENTED_EDGE ( 'NONE', *, *, #2307, .F. ) ;
#5070 = DIRECTION ( 'NONE',  ( -0.9876526153536336894, -0.1566598588826349503, 0.000000000000000000 ) ) ;
#5071 = CARTESIAN_POINT ( 'NONE',  ( 0.000000000000000000, 0.000000000000000000, -35.00000000000000000 ) ) ;
#5072 = DIRECTION ( 'NONE',  ( -0.000000000000000000, -0.000000000000000000, -1.000000000000000000 ) ) ;
#5073 = CARTESIAN_POINT ( 'NONE',  ( -32.22008523532134205, -25.36048350923618955, 4.330127018922217630 ) ) ;
#5074 = SURFACE_STYLE_USAGE ( .BOTH. , #13996 ) ;
#5075 = DIRECTION ( 'NONE',  ( -0.9876526153536341335, -0.1566598588826327021, 0.000000000000000000 ) ) ;
#5076 = EDGE_CURVE ( 'NONE', #5608, #14700, #12187, .T. ) ;
#5078 = CARTESIAN_POINT ( 'NONE',  ( -41.56315007100294423, -84.54793360496931598, 12.99038105676661203 ) ) ;
#5077 = VECTOR ( 'NONE', #6211, 999.9999999999998863 ) ;
#5079 = AXIS2_PLACEMENT_3D ( 'NONE', #14440, #18754, #1294 ) ;
#5080 = CARTESIAN_POINT ( 'NONE',  ( -68.72359699322777260, -88.85607972424168111, -8.660254037844385522 ) ) ;
#5081 = ORIENTED_EDGE ( 'NONE', *, *, #1319, .F. ) ;
#5082 = CARTESIAN_POINT ( 'NONE',  ( 73.09088021254186174, 1.387778780781445676E-14, -7.500000000000000000 ) ) ;
#5083 = EDGE_CURVE ( 'NONE', #6519, #9513, #9949, .T. ) ;
#5084 = FACE_OUTER_BOUND ( 'NONE', #4717, .T. ) ;
#5086 = ORIENTED_EDGE ( 'NONE', *, *, #11457, .F. ) ;
#5085 = CARTESIAN_POINT ( 'NONE',  ( -16.70711637639958269, -17.83733276090463704, 12.99038105676661381 ) ) ;
#5087 =( GEOMETRIC_REPRESENTATION_CONTEXT ( 3 ) GLOBAL_UNCERTAINTY_ASSIGNED_CONTEXT ( ( #580 ) ) GLOBAL_UNIT_ASSIGNED_CONTEXT ( ( #14853, #15036, #17648 ) ) REPRESENTATION_CONTEXT ( 'NONE', 'WORKASPACE' ) );
#5088 = EDGE_CURVE ( 'NONE', #3468, #14246, #16640, .T. ) ;
#5089 = DIRECTION ( 'NONE',  ( -0.9876526153536341335, -0.1566598588826327021, 0.000000000000000000 ) ) ;
#5090 = EDGE_CURVE ( 'NONE', #8278, #15183, #591, .T. ) ;
#5091 = ORIENTED_EDGE ( 'NONE', *, *, #10771, .T. ) ;
#5092 = ORIENTED_EDGE ( 'NONE', *, *, #17409, .F. ) ;
#5094 = VECTOR ( 'NONE', #9866, 1000.000000000000000 ) ;
#5093 = LINE ( 'NONE', #10867, #3904 ) ;
#5095 = LINE ( 'NONE', #8038, #296 ) ;
#5096 = AXIS2_PLACEMENT_3D ( 'NONE', #7416, #10519, #6283 ) ;
#5097 = DIRECTION ( 'NONE',  ( 1.000000000000000000, 0.000000000000000000, 0.000000000000000000 ) ) ;
#5098 = ORIENTED_EDGE ( 'NONE', *, *, #6813, .T. ) ;
#5099 = CIRCLE ( 'NONE', #8737, 1.500000000000001332 ) ;
#5100 = LINE ( 'NONE', #8042, #9467 ) ;
#5101 = CIRCLE ( 'NONE', #7834, 12.74754878398197633 ) ;
#5102 = DIRECTION ( 'NONE',  ( -0.1566598588826321192, 0.9876526153536342445, 7.798540720466730171E-17 ) ) ;
#5103 = DIRECTION ( 'NONE',  ( 1.000000000000000000, 0.000000000000000000, 0.000000000000000000 ) ) ;
#5104 = DIRECTION ( 'NONE',  ( -0.1566598588826321192, 0.9876526153536342445, 7.798540720466731404E-17 ) ) ;
#5105 = CARTESIAN_POINT ( 'NONE',  ( -68.76323200340561925, -31.15689828789355786, -21.65063509461098334 ) ) ;
#5106 = CARTESIAN_POINT ( 'NONE',  ( -78.43540483600145308, -27.62857394106912423, 17.32050807568882078 ) ) ;
#5107 = CARTESIAN_POINT ( 'NONE',  ( -42.87991068327079347, -21.98881902129436838, -21.65063509461098334 ) ) ;
#5108 = VERTEX_POINT ( 'NONE', #15146 ) ;
#5109 = CIRCLE ( 'NONE', #9363, 1.500000000000000444 ) ;
#5110 = LINE ( 'NONE', #585, #7648 ) ;
#5111 = DIRECTION ( 'NONE',  ( -0.1566598588826321747, 0.9876526153536343555, 0.000000000000000000 ) ) ;
#5112 = AXIS2_PLACEMENT_3D ( 'NONE', #14114, #5515, #11270 ) ;
#5113 = AXIS2_PLACEMENT_3D ( 'NONE', #15886, #11778, #4600 ) ;
#5114 = EDGE_CURVE ( 'NONE', #1113, #202, #2991, .T. ) ;
#5115 = DIRECTION ( 'NONE',  ( 8.693966348389027220E-17, -1.991237296706374949E-16, 1.000000000000000000 ) ) ;
#5116 = VECTOR ( 'NONE', #914, 1000.000000000000000 ) ;
#5117 = VECTOR ( 'NONE', #14676, 1000.000000000000227 ) ;
#5118 = VECTOR ( 'NONE', #16253, 1000.000000000000114 ) ;
#5119 = ORIENTED_EDGE ( 'NONE', *, *, #13310, .F. ) ;
#5120 = ORIENTED_EDGE ( 'NONE', *, *, #13738, .F. ) ;
#5121 = ORIENTED_EDGE ( 'NONE', *, *, #7378, .F. ) ;
#5122 = CYLINDRICAL_SURFACE ( 'NONE', #16539, 1.500000000000001554 ) ;
#5123 = EDGE_LOOP ( 'NONE', ( #15285, #4770, #3531, #17351 ) ) ;
#5124 = FACE_BOUND ( 'NONE', #17158, .T. ) ;
#5125 = EDGE_CURVE ( 'NONE', #1703, #8251, #13579, .T. ) ;
#5126 = CIRCLE ( 'NONE', #3297, 1.500000000000001332 ) ;
#5127 = AXIS2_PLACEMENT_3D ( 'NONE', #12925, #14286, #5471 ) ;
#5128 = EDGE_CURVE ( 'NONE', #17749, #11803, #14388, .T. ) ;
#5129 = AXIS2_PLACEMENT_3D ( 'NONE', #12225, #9502, #16515 ) ;
#5130 = AXIS2_PLACEMENT_3D ( 'NONE', #8094, #16749, #5450 ) ;
#5131 = CIRCLE ( 'NONE', #18205, 2.500000000000002220 ) ;
#5132 = ORIENTED_EDGE ( 'NONE', *, *, #12297, .T. ) ;
#5133 = DIRECTION ( 'NONE',  ( 0.000000000000000000, 0.000000000000000000, 1.000000000000000000 ) ) ;
#5134 = ORIENTED_EDGE ( 'NONE', *, *, #12741, .T. ) ;
#5135 = CARTESIAN_POINT ( 'NONE',  ( -60.36818477289978091, -29.82528948739120267, -12.99038105676658006 ) ) ;
#5136 = ORIENTED_EDGE ( 'NONE', *, *, #14044, .T. ) ;
#5137 = FACE_OUTER_BOUND ( 'NONE', #13046, .T. ) ;
#5138 = CARTESIAN_POINT ( 'NONE',  ( -71.72618984946653597, -31.62687786454144856, -21.65063509461098334 ) ) ;
#5139 = AXIS2_PLACEMENT_3D ( 'NONE', #15398, #15435, #18520 ) ;
#5140 = CARTESIAN_POINT ( 'NONE',  ( -50.49165861936347710, -28.25869089856488614, -4.330127018922181215 ) ) ;
#5141 = ORIENTED_EDGE ( 'NONE', *, *, #17517, .T. ) ;
#5142 = ORIENTED_EDGE ( 'NONE', *, *, #10711, .T. ) ;
#5143 = DIRECTION ( 'NONE',  ( 1.000000000000000000, 0.000000000000000000, 0.000000000000000000 ) ) ;
#5144 = CARTESIAN_POINT ( 'NONE',  ( -306.1404785418517918, -2.850701963179328668, 12.83663829214476237 ) ) ;
#5145 = VECTOR ( 'NONE', #2578, 1000.000000000000114 ) ;
#5146 = DIRECTION ( 'NONE',  ( 0.000000000000000000, 0.000000000000000000, 1.000000000000000000 ) ) ;
#5147 = ORIENTED_EDGE ( 'NONE', *, *, #11792, .F. ) ;
#5148 = VERTEX_POINT ( 'NONE', #8414 ) ;
#5149 = CIRCLE ( 'NONE', #12405, 1.500000000000001332 ) ;
#5150 = CARTESIAN_POINT ( 'NONE',  ( -18.39294862037050393, -23.16724548487935564, -8.660254037844380193 ) ) ;
#5151 = ORIENTED_EDGE ( 'NONE', *, *, #6193, .F. ) ;
#5152 = VERTEX_POINT ( 'NONE', #7113 ) ;
#5153 = ORIENTED_EDGE ( 'NONE', *, *, #5243, .F. ) ;
#5154 = CARTESIAN_POINT ( 'NONE',  ( -127.5060788346647200, -15.25314381392001728, 2.821239268406352974 ) ) ;
#5155 = ADVANCED_FACE ( 'NONE', ( #12941 ), #12656, .F. ) ;
#5156 = DIRECTION ( 'NONE',  ( -0.9876526153536336894, -0.1566598588826349503, 0.000000000000000000 ) ) ;
#5157 = CARTESIAN_POINT ( 'NONE',  ( 6.338001773648100468, -76.94993044916168401, 21.65063509461100821 ) ) ;
#5158 = EDGE_CURVE ( 'NONE', #93, #4467, #15107, .T. ) ;
#5159 = FACE_BOUND ( 'NONE', #1486, .T. ) ;
#5160 = VECTOR ( 'NONE', #12833, 1000.000000000000000 ) ;
#5161 = LINE ( 'NONE', #9519, #8195 ) ;
#5162 = ADVANCED_FACE ( 'NONE', ( #13041 ), #2992, .F. ) ;
#5163 = CIRCLE ( 'NONE', #18227, 5.000000000000000000 ) ;
#5164 = CARTESIAN_POINT ( 'NONE',  ( -62.83731631128386397, -30.21693913459777647, -8.660254037844380193 ) ) ;
#5165 = CARTESIAN_POINT ( 'NONE',  ( -70.15002351626573329, 45.06383568389368577, 6.194099995621382249 ) ) ;
#5166 = SURFACE_SIDE_STYLE ('',( #12339 ) ) ;
#5167 = CARTESIAN_POINT ( 'NONE',  ( 2.881217619910392269, -77.49823995525089515, -21.65063509461098690 ) ) ;
#5168 = VECTOR ( 'NONE', #3159, 1000.000000000000000 ) ;
#5169 = CARTESIAN_POINT ( 'NONE',  ( -38.92930022185625205, -21.36217958576383680, 1.214306433183764966E-14 ) ) ;
#5170 = CARTESIAN_POINT ( 'NONE',  ( -15.39035576413176187, -80.39644734457957043, -4.330127018922185655 ) ) ;
#5171 = AXIS2_PLACEMENT_3D ( 'NONE', #2811, #12838, #12923 ) ;
#5172 = CYLINDRICAL_SURFACE ( 'NONE', #6520, 1.500000000000001554 ) ;
#5173 = ORIENTED_EDGE ( 'NONE', *, *, #4933, .T. ) ;
#5174 = EDGE_LOOP ( 'NONE', ( #7389, #2368 ) ) ;
#5175 = DIRECTION ( 'NONE',  ( -0.1566598588826321192, 0.9876526153536342445, 7.798540720466730171E-17 ) ) ;
#5176 = ORIENTED_EDGE ( 'NONE', *, *, #8295, .T. ) ;
#5177 = CIRCLE ( 'NONE', #10308, 1.500000000000000888 ) ;
#5178 = CARTESIAN_POINT ( 'NONE',  ( -72.71384246482016067, -31.78353772342409300, -17.32050807568878170 ) ) ;
#5179 = CIRCLE ( 'NONE', #10016, 20.00000000000001066 ) ;
#5180 = EDGE_LOOP ( 'NONE', ( #373, #17700 ) ) ;
#5181 = DIRECTION ( 'NONE',  ( -0.1566598588826321192, 0.9876526153536342445, 7.798540720466730171E-17 ) ) ;
#5182 = CARTESIAN_POINT ( 'NONE',  ( -51.43967622453925514, -86.11453219379563961, 12.99038105676661203 ) ) ;
#5183 = AXIS2_PLACEMENT_3D ( 'NONE', #5150, #9423, #3992 ) ;
#5184 = CARTESIAN_POINT ( 'NONE',  ( -55.42992169613163611, -29.04199019297804085, -12.99038105676658006 ) ) ;
#5185 = DIRECTION ( 'NONE',  ( -0.1566598588826321192, 0.9876526153536342445, 7.798540720466731404E-17 ) ) ;
#5186 = AXIS2_PLACEMENT_3D ( 'NONE', #9044, #17986, #4676 ) ;
#5187 = EDGE_LOOP ( 'NONE', ( #16418, #5453, #16871, #7830 ) ) ;
#5188 = CYLINDRICAL_SURFACE ( 'NONE', #9410, 1.500000000000001554 ) ;
#5189 = EDGE_CURVE ( 'NONE', #7443, #8527, #10273, .T. ) ;
#5190 = LINE ( 'NONE', #11133, #16787 ) ;
#5191 = VERTEX_POINT ( 'NONE', #1409 ) ;
#5192 = CYLINDRICAL_SURFACE ( 'NONE', #14296, 1.500000000000001554 ) ;
#5193 = CIRCLE ( 'NONE', #8224, 1.500000000000000000 ) ;
#5194 = CIRCLE ( 'NONE', #16084, 1.999999999999998224 ) ;
#5195 = DIRECTION ( 'NONE',  ( -0.1566598588826321747, 0.9876526153536343555, 0.000000000000000000 ) ) ;
#5196 = CARTESIAN_POINT ( 'NONE',  ( -26.74836084069850983, -82.19803572172985184, 4.330127018922213189 ) ) ;
#5197 = ADVANCED_FACE ( 'NONE', ( #4035 ), #12767, .F. ) ;
#5198 = CYLINDRICAL_SURFACE ( 'NONE', #3247, 1.500000000000000666 ) ;
#5199 = AXIS2_PLACEMENT_3D ( 'NONE', #4914, #12000, #5103 ) ;
#5200 = CARTESIAN_POINT ( 'NONE',  ( -25.59598991458226536, -19.24727149084831623, -17.32050807568878170 ) ) ;
#5201 = CARTESIAN_POINT ( 'NONE',  ( -68.72359699322777260, -88.85607972424169532, 17.32050807568881368 ) ) ;
#5203 = VERTEX_POINT ( 'NONE', #10105 ) ;
#5202 = CARTESIAN_POINT ( 'NONE',  ( -21.64537945316773460, -18.62063205531779175, -21.65063509461097979 ) ) ;
#5204 = AXIS2_PLACEMENT_3D ( 'NONE', #18644, #5707, #17185 ) ;
#5205 = DIRECTION ( 'NONE',  ( 0.000000000000000000, 0.000000000000000000, 1.000000000000000000 ) ) ;
#5206 = CYLINDRICAL_SURFACE ( 'NONE', #25, 1.500000000000000666 ) ;
#5207 = ORIENTED_EDGE ( 'NONE', *, *, #3058, .T. ) ;
#5208 = VECTOR ( 'NONE', #11210, 1000.000000000000000 ) ;
#5209 =( REPRESENTATION_RELATIONSHIP ('NONE','NONE', #7353, #10585 ) REPRESENTATION_RELATIONSHIP_WITH_TRANSFORMATION ( #18480 )SHAPE_REPRESENTATION_RELATIONSHIP( ) );
#5210 = DIRECTION ( 'NONE',  ( -0.1566598588826321747, 0.9876526153536343555, 0.000000000000000000 ) ) ;
#5211 = CARTESIAN_POINT ( 'NONE',  ( -26.58364252993588650, -19.40393134973096068, 12.99038105676661736 ) ) ;
#5212 = CARTESIAN_POINT ( 'NONE',  ( -129.0020721423141481, 9.044883704321415863, -4.579216830445306030 ) ) ;
#5213 = ORIENTED_EDGE ( 'NONE', *, *, #1947, .T. ) ;
#5214 = CARTESIAN_POINT ( 'NONE',  ( -67.77557938805200877, -31.00023842901093118, 17.32050807568881723 ) ) ;
#5215 = CARTESIAN_POINT ( 'NONE',  ( -39.13365354279673625, -26.45710252141460828, -21.65063509461098334 ) ) ;
#5216 = EDGE_CURVE ( 'NONE', #3364, #5781, #1503, .T. ) ;
#5217 = EDGE_CURVE ( 'NONE', #9201, #15912, #4213, .T. ) ;
#5218 = LINE ( 'NONE', #6645, #11724 ) ;
#5219 = FACE_OUTER_BOUND ( 'NONE', #10013, .T. ) ;
#5220 = DIRECTION ( 'NONE',  ( -0.1566598588826321192, 0.9876526153536342445, 7.798540720466730171E-17 ) ) ;
#5221 = CYLINDRICAL_SURFACE ( 'NONE', #15011, 150.0000000000000000 ) ;
#5222 = ORIENTED_EDGE ( 'NONE', *, *, #9229, .T. ) ;
#5223 = EDGE_CURVE ( 'NONE', #11862, #3864, #2062, .T. ) ;
#5224 = DIRECTION ( 'NONE',  ( 0.000000000000000000, 0.000000000000000000, 1.000000000000000000 ) ) ;
#5225 = DIRECTION ( 'NONE',  ( -0.1566598588826321192, 0.9876526153536342445, 7.798540720466731404E-17 ) ) ;
#5226 = CARTESIAN_POINT ( 'NONE',  ( -16.87183468716221313, -80.63143713290352821, 4.330127018922213189 ) ) ;
#5227 = AXIS2_PLACEMENT_3D ( 'NONE', #15553, #8354, #5326 ) ;
#5228 = ORIENTED_EDGE ( 'NONE', *, *, #11524, .T. ) ;
#5229 = AXIS2_PLACEMENT_3D ( 'NONE', #126, #14147, #4081 ) ;
#5230 = VERTEX_POINT ( 'NONE', #8522 ) ;
#5231 = EDGE_LOOP ( 'NONE', ( #15894, #11648 ) ) ;
#5232 = DIRECTION ( 'NONE',  ( -0.000000000000000000, -0.000000000000000000, -1.000000000000000000 ) ) ;
#5233 = FACE_BOUND ( 'NONE', #3960, .T. ) ;
#5234 = DIRECTION ( 'NONE',  ( -0.9876526153536341335, -0.1566598588826327021, 0.000000000000000000 ) ) ;
#5235 = ORIENTED_EDGE ( 'NONE', *, *, #10858, .F. ) ;
#5236 = EDGE_CURVE ( 'NONE', #7636, #17961, #14298, .T. ) ;
#5237 = CIRCLE ( 'NONE', #9784, 1.500000000000000888 ) ;
#5238 = ORIENTED_EDGE ( 'NONE', *, *, #14131, .T. ) ;
#5239 = CARTESIAN_POINT ( 'NONE',  ( -63.62061560569701157, -25.27867605782963523, -17.32050807568878170 ) ) ;
#5240 = ORIENTED_EDGE ( 'NONE', *, *, #4437, .F. ) ;
#5241 = DIRECTION ( 'NONE',  ( -0.1566598588826321192, 0.9876526153536342445, 7.798540720466730171E-17 ) ) ;
#5242 = DIRECTION ( 'NONE',  ( -0.1566598588826321192, 0.9876526153536342445, 7.798540720466730171E-17 ) ) ;
#5243 = EDGE_CURVE ( 'NONE', #755, #1263, #11767, .T. ) ;
#5244 = LINE ( 'NONE', #18273, #2594 ) ;
#5245 = ORIENTED_EDGE ( 'NONE', *, *, #18253, .T. ) ;
#5246 = FACE_OUTER_BOUND ( 'NONE', #12849, .T. ) ;
#5247 = ORIENTED_EDGE ( 'NONE', *, *, #13225, .T. ) ;
#5248 = FACE_OUTER_BOUND ( 'NONE', #15637, .T. ) ;
#5249 = VERTEX_POINT ( 'NONE', #16805 ) ;
#5250 = VERTEX_POINT ( 'NONE', #2473 ) ;
#5251 = CARTESIAN_POINT ( 'NONE',  ( 3.000000000000000000, 0.000000000000000000, 32.00000000000000000 ) ) ;
#5252 = CIRCLE ( 'NONE', #14026, 1.500000000000000888 ) ;
#5253 = FACE_OUTER_BOUND ( 'NONE', #5034, .T. ) ;
#5254 = CARTESIAN_POINT ( 'NONE',  ( -128.1659926135409933, -15.15280585534915225, 3.278196957010496959 ) ) ;
#5255 = CARTESIAN_POINT ( 'NONE',  ( -0.9046745307415022808, -15.33077501878252136, -17.32050807568878170 ) ) ;
#5256 = ORIENTED_EDGE ( 'NONE', *, *, #394, .T. ) ;
#5257 = CARTESIAN_POINT ( 'NONE',  ( -138.4775067298212718, -42.93618108924343346, 2.500000000000000000 ) ) ;
#5258 = CYLINDRICAL_SURFACE ( 'NONE', #16659, 1.500000000000000888 ) ;
#5259 = CARTESIAN_POINT ( 'NONE',  ( -3.044698072211382112, -78.43819910854666944, -17.32050807568878525 ) ) ;
#5260 = DIRECTION ( 'NONE',  ( 0.000000000000000000, 0.000000000000000000, 1.000000000000000000 ) ) ;
#5261 = CIRCLE ( 'NONE', #10986, 2.000000000000001776 ) ;
#5262 = DIRECTION ( 'NONE',  ( 0.000000000000000000, 0.000000000000000000, 1.000000000000000000 ) ) ;
#5263 = DIRECTION ( 'NONE',  ( -0.1566598588826321747, 0.9876526153536343555, 0.000000000000000000 ) ) ;
#5264 = EDGE_CURVE ( 'NONE', #14963, #13690, #17575, .T. ) ;
#5265 = CYLINDRICAL_SURFACE ( 'NONE', #9028, 1.500000000000000666 ) ;
#5266 = CARTESIAN_POINT ( 'NONE',  ( -105.9742111339482307, -32.54855632894931716, 2.500000000000000000 ) ) ;
#5267 = ORIENTED_EDGE ( 'NONE', *, *, #2782, .F. ) ;
#5268 = ADVANCED_FACE ( 'NONE', ( #12203 ), #6554, .F. ) ;
#5269 = ORIENTED_EDGE ( 'NONE', *, *, #10087, .F. ) ;
#5270 = DIRECTION ( 'NONE',  ( -0.1566598588826321192, 0.9876526153536342445, 7.798540720466730171E-17 ) ) ;
#5271 = VERTEX_POINT ( 'NONE', #5313 ) ;
#5272 = ORIENTED_EDGE ( 'NONE', *, *, #18701, .F. ) ;
#5273 = ORIENTED_EDGE ( 'NONE', *, *, #16069, .T. ) ;
#5274 = EDGE_CURVE ( 'NONE', #16906, #18093, #14225, .T. ) ;
#5275 = DIRECTION ( 'NONE',  ( -0.1566598588826321192, 0.9876526153536342445, 7.798540720466730171E-17 ) ) ;
#5276 = ORIENTED_EDGE ( 'NONE', *, *, #2289, .T. ) ;
#5277 = CARTESIAN_POINT ( 'NONE',  ( -67.24211807019732134, -88.62108993591773753, -8.660254037844385522 ) ) ;
#5278 = DIRECTION ( 'NONE',  ( -0.1566598588826321192, 0.9876526153536342445, 7.798540720466730171E-17 ) ) ;
#5279 = DIRECTION ( 'NONE',  ( 1.000000000000000000, 0.000000000000000000, 0.000000000000000000 ) ) ;
#5280 = VERTEX_POINT ( 'NONE', #8261 ) ;
#5281 = CARTESIAN_POINT ( 'NONE',  ( -16.87183468716221313, -80.63143713290354242, 21.65063509461101532 ) ) ;
#5282 = CARTESIAN_POINT ( 'NONE',  ( -1.109027851681966492, -20.42569795443330349, 21.65063509461101177 ) ) ;
#5283 = DIRECTION ( 'NONE',  ( -0.9876526153536336894, -0.1566598588826349503, 0.000000000000000000 ) ) ;
#5284 =( NAMED_UNIT ( * ) PLANE_ANGLE_UNIT ( ) SI_UNIT ( $, .RADIAN. ) );
#5285 = ORIENTED_EDGE ( 'NONE', *, *, #12389, .F. ) ;
#5286 = CARTESIAN_POINT ( 'NONE',  ( -20.32861884089991023, -81.17974663899272514, -4.330127018922185655 ) ) ;
#5287 = EDGE_LOOP ( 'NONE', ( #593, #15852 ) ) ;
#5288 = DIRECTION ( 'NONE',  ( -0.1566598588826321192, 0.9876526153536342445, 7.798540720466731404E-17 ) ) ;
#5289 = FACE_OUTER_BOUND ( 'NONE', #13039, .T. ) ;
#5290 = DIRECTION ( 'NONE',  ( -0.9876526153536336894, -0.1566598588826349503, 0.000000000000000000 ) ) ;
#5291 = CARTESIAN_POINT ( 'NONE',  ( -76.89394439365321432, -2.165653619537352803, 7.122830718932430472 ) ) ;
#5293 = ORIENTED_EDGE ( 'NONE', *, *, #15041, .F. ) ;
#5292 = CARTESIAN_POINT ( 'NONE',  ( 3.231158466157545206, -19.73726462726228092, 30.00000000000000000 ) ) ;
#5294 = DIRECTION ( 'NONE',  ( -0.1566598588826321192, 0.9876526153536342445, 7.798540720466730171E-17 ) ) ;
#5295 = EDGE_CURVE ( 'NONE', #1415, #2898, #6053, .T. ) ;
#5296 = AXIS2_PLACEMENT_3D ( 'NONE', #9960, #15756, #2776 ) ;
#5297 = ORIENTED_EDGE ( 'NONE', *, *, #3696, .T. ) ;
#5298 = ORIENTED_EDGE ( 'NONE', *, *, #4886, .T. ) ;
#5299 = EDGE_LOOP ( 'NONE', ( #2856, #14891 ) ) ;
#5300 = DIRECTION ( 'NONE',  ( -0.1566598588826321192, 0.9876526153536342445, 7.798540720466731404E-17 ) ) ;
#5301 = DIRECTION ( 'NONE',  ( 0.000000000000000000, 0.000000000000000000, 1.000000000000000000 ) ) ;
#5302 = EDGE_CURVE ( 'NONE', #12897, #370, #8764, .T. ) ;
#5303 = CYLINDRICAL_SURFACE ( 'NONE', #15136, 1.500000000000001554 ) ;
#5304 = CYLINDRICAL_SURFACE ( 'NONE', #17373, 1.500000000000000666 ) ;
#5305 = EDGE_CURVE ( 'NONE', #6856, #18075, #4523, .T. ) ;
#5306 = PLANE ( 'NONE',  #7037 ) ;
#5307 = CARTESIAN_POINT ( 'NONE',  ( -0.5755665338273089349, -78.04654946134009208, -12.99038105676658539 ) ) ;
#5308 = DIRECTION ( 'NONE',  ( -0.1566598588826321747, 0.9876526153536343555, 0.000000000000000000 ) ) ;
#5309 = DIRECTION ( 'NONE',  ( -0.1566598588826321192, 0.9876526153536342445, 7.798540720466730171E-17 ) ) ;
#5310 = AXIS2_PLACEMENT_3D ( 'NONE', #4684, #10466, #13316 ) ;
#5311 = CARTESIAN_POINT ( 'NONE',  ( -126.9394941819792280, 9.589416411885151703, -2.601363783521511763 ) ) ;
#5312 = DIRECTION ( 'NONE',  ( -0.1566598588826321192, 0.9876526153536342445, 7.798540720466730171E-17 ) ) ;
#5313 = CARTESIAN_POINT ( 'NONE',  ( -61.35583738825339850, -29.98194934627382224, 17.32050807568881723 ) ) ;
#5314 = ORIENTED_EDGE ( 'NONE', *, *, #55, .T. ) ;
#5315 = VERTEX_POINT ( 'NONE', #15541 ) ;
#5316 =( REPRESENTATION_RELATIONSHIP ('NONE','NONE', #7353, #15677 ) REPRESENTATION_RELATIONSHIP_WITH_TRANSFORMATION ( #4095 )SHAPE_REPRESENTATION_RELATIONSHIP( ) );
#5317 = CARTESIAN_POINT ( 'NONE',  ( -41.39843176024032800, -21.75382923297043902, 21.65063509461102242 ) ) ;
#5318 = EDGE_CURVE ( 'NONE', #2138, #18388, #9390, .T. ) ;
#5319 = ORIENTED_EDGE ( 'NONE', *, *, #18794, .F. ) ;
#5320 = ORIENTED_EDGE ( 'NONE', *, *, #18052, .F. ) ;
#5321 = CARTESIAN_POINT ( 'NONE',  ( -17.69476899175320739, -17.99399261978726727, -17.32050807568878170 ) ) ;
#5322 = EDGE_CURVE ( 'NONE', #11461, #5108, #16920, .T. ) ;
#5323 = FACE_BOUND ( 'NONE', #18165, .T. ) ;
#5324 = ADVANCED_FACE ( 'NONE', ( #7314 ), #13065, .T. ) ;
#5325 = CARTESIAN_POINT ( 'NONE',  ( 10.28861223506262412, -76.32329101363113466, -17.32050807568878525 ) ) ;
#5326 = DIRECTION ( 'NONE',  ( -0.9876526153536336894, -0.1566598588826350336, 0.000000000000000000 ) ) ;
#5327 = ORIENTED_EDGE ( 'NONE', *, *, #5083, .F. ) ;
#5328 = DIRECTION ( 'NONE',  ( -0.1566598588826321192, 0.9876526153536342445, 7.798540720466731404E-17 ) ) ;
#5329 = LINE ( 'NONE', #1362, #14099 ) ;
#5330 = DIRECTION ( 'NONE',  ( -0.9876526153536336894, -0.1566598588826349503, 0.000000000000000000 ) ) ;
#5331 = VECTOR ( 'NONE', #15348, 1000.000000000000000 ) ;
#5332 = CARTESIAN_POINT ( 'NONE',  ( -35.14340807120434818, -83.52964452223221770, 4.330127018922213189 ) ) ;
#5333 = DIRECTION ( 'NONE',  ( -0.1566598588826321192, 0.9876526153536342445, 7.798540720466730171E-17 ) ) ;
#5334 = CARTESIAN_POINT ( 'NONE',  ( -45.51376053241749986, -85.17457304049983691, -8.660254037844385522 ) ) ;
#5335 = ORIENTED_EDGE ( 'NONE', *, *, #7026, .F. ) ;
#5336 = DIRECTION ( 'NONE',  ( -0.1566598588826321192, 0.9876526153536342445, 7.798540720466730171E-17 ) ) ;
#5337 = EDGE_CURVE ( 'NONE', #983, #17992, #16331, .T. ) ;
#5338 = DIRECTION ( 'NONE',  ( -0.9876526153536341335, -0.1566598588826327021, 0.000000000000000000 ) ) ;
#5339 = EDGE_CURVE ( 'NONE', #12633, #6562, #3896, .T. ) ;
#5340 = CARTESIAN_POINT ( 'NONE',  ( -167.4745151998187680, 32.15905408292206147, -2.500000000000000000 ) ) ;
#5341 = ORIENTED_EDGE ( 'NONE', *, *, #11337, .T. ) ;
#5342 = ORIENTED_EDGE ( 'NONE', *, *, #8909, .F. ) ;
#5343 = CARTESIAN_POINT ( 'NONE',  ( -51.47931123471709469, -28.41535075744750571, 17.32050807568881723 ) ) ;
#5344 = EDGE_CURVE ( 'NONE', #14700, #18093, #6409, .T. ) ;
#5345 = EDGE_CURVE ( 'NONE', #12027, #18395, #6941, .T. ) ;
#5346 = AXIS2_PLACEMENT_3D ( 'NONE', #2098, #15176, #693 ) ;
#5347 = EDGE_LOOP ( 'NONE', ( #11218, #9334 ) ) ;
#5348 = ORIENTED_EDGE ( 'NONE', *, *, #16081, .T. ) ;
#5349 = CARTESIAN_POINT ( 'NONE',  ( -128.5628356445764098, -15.03429919720559482, 3.719291248522907711 ) ) ;
#5350 = DIRECTION ( 'NONE',  ( -0.1566598588826321192, 0.9876526153536342445, 7.798540720466730171E-17 ) ) ;
#5351 = EDGE_CURVE ( 'NONE', #9530, #8822, #14522, .T. ) ;
#5352 = AXIS2_PLACEMENT_3D ( 'NONE', #6727, #18413, #9649 ) ;
#5353 = CARTESIAN_POINT ( 'NONE',  ( 0.000000000000000000, 0.000000000000000000, -30.00000000000000000 ) ) ;
#5354 = CARTESIAN_POINT ( 'NONE',  ( -73.14061779976039190, 46.33634706135890013, 2.761024190134958811 ) ) ;
#5355 = VECTOR ( 'NONE', #5879, 1000.000000000000000 ) ;
#5356 = AXIS2_PLACEMENT_3D ( 'NONE', #4813, #17834, #10501 ) ;
#5357 = ADVANCED_FACE ( 'NONE', ( #8714 ), #1523, .F. ) ;
#5358 = CARTESIAN_POINT ( 'NONE',  ( -71.02801022084922522, -26.45362499944938861, 21.65063509461102242 ) ) ;
#5359 = CARTESIAN_POINT ( 'NONE',  ( -2.590506774712417748, -20.66068774275724707, -4.330127018922184767 ) ) ;
#5360 = ADVANCED_FACE ( 'NONE', ( #16007 ), #9939, .F. ) ;
#5361 = CARTESIAN_POINT ( 'NONE',  ( 9.300959619709004755, -76.47995087251376845, 4.330127018922207860 ) ) ;
#5362 = VERTEX_POINT ( 'NONE', #2751 ) ;
#5363 = ORIENTED_EDGE ( 'NONE', *, *, #12144, .F. ) ;
#5364 = DIRECTION ( 'NONE',  ( 1.000000000000000000, 0.000000000000000000, -3.469446951953612217E-16 ) ) ;
#5365 = VECTOR ( 'NONE', #3530, 1000.000000000000000 ) ;
#5366 = VERTEX_POINT ( 'NONE', #18718 ) ;
#5367 = CIRCLE ( 'NONE', #840, 1.500000000000000888 ) ;
#5368 = ORIENTED_EDGE ( 'NONE', *, *, #17030, .T. ) ;
#5369 = AXIS2_PLACEMENT_3D ( 'NONE', #832, #6808, #18099 ) ;
#5370 = ORIENTED_EDGE ( 'NONE', *, *, #6948, .T. ) ;
#5371 = CARTESIAN_POINT ( 'NONE',  ( -11.76885329963143079, -17.05403346649147878, 12.99038105676661381 ) ) ;
#5372 = AXIS2_PLACEMENT_3D ( 'NONE', #5919, #17498, #4583 ) ;
#5373 = CARTESIAN_POINT ( 'NONE',  ( -3.000000000000000000, 0.000000000000000000, -37.00000000000000711 ) ) ;
#5374 = EDGE_CURVE ( 'NONE', #6411, #16333, #15117, .T. ) ;
#5375 = ORIENTED_EDGE ( 'NONE', *, *, #5351, .T. ) ;
#5376 = DIRECTION ( 'NONE',  ( 1.000000000000000000, 0.000000000000000000, 0.000000000000000000 ) ) ;
#5377 = EDGE_CURVE ( 'NONE', #12139, #10552, #12374, .T. ) ;
#5378 = DIRECTION ( 'NONE',  ( 1.000000000000000000, 0.000000000000000000, 0.000000000000000000 ) ) ;
#5379 = CARTESIAN_POINT ( 'NONE',  ( -39.91695283720989096, -21.51883944464647769, -21.65063509461098334 ) ) ;
#5380 = AXIS2_PLACEMENT_3D ( 'NONE', #4588, #331, #16523 ) ;
#5381 = ORIENTED_EDGE ( 'NONE', *, *, #12963, .T. ) ;
#5382 = CARTESIAN_POINT ( 'NONE',  ( -49.59961335071796640, 39.40051552679454971, 20.00000000000001066 ) ) ;
#5383 = ORIENTED_EDGE ( 'NONE', *, *, #5544, .T. ) ;
#5384 = CYLINDRICAL_SURFACE ( 'NONE', #197, 1.500000000000000666 ) ;
#5385 = VECTOR ( 'NONE', #16974, 1000.000000000000000 ) ;
#5386 = CARTESIAN_POINT ( 'NONE',  ( -82.39751269876940398, 30.59191086097347778, 35.00001199999999812 ) ) ;
#5387 = LINE ( 'NONE', #11145, #5385 ) ;
#5389 = EDGE_LOOP ( 'NONE', ( #7582, #9462 ) ) ;
#5388 = CARTESIAN_POINT ( 'NONE',  ( 0.4120860815263194254, -77.88988960245745830, 17.32050807568880657 ) ) ;
#5390 = DIRECTION ( 'NONE',  ( -0.1566598588826321192, 0.9876526153536342445, 7.798540720466731404E-17 ) ) ;
#5391 = ORIENTED_EDGE ( 'NONE', *, *, #7845, .T. ) ;
#5392 = AXIS2_PLACEMENT_3D ( 'NONE', #481, #14785, #16496 ) ;
#5393 = ORIENTED_EDGE ( 'NONE', *, *, #7421, .F. ) ;
#5394 = ORIENTED_EDGE ( 'NONE', *, *, #8911, .T. ) ;
#5395 = CARTESIAN_POINT ( 'NONE',  ( -24.11451099155181055, -19.01228170252437977, 8.660254037844417496 ) ) ;
#5396 = VERTEX_POINT ( 'NONE', #4624 ) ;
#5397 = SHAPE_REPRESENTATION ( 'Upper Squeezer Handle Arm', ( #18772 ), #18155 ) ;
#5398 = CARTESIAN_POINT ( 'NONE',  ( -49.01017969633302584, -28.02370111024093191, -4.330127018922181215 ) ) ;
#5399 = CARTESIAN_POINT ( 'NONE',  ( -35.47251606811855851, -20.81387007967463276, -17.32050807568878170 ) ) ;
#5400 = CARTESIAN_POINT ( 'NONE',  ( -81.37351714223066779, 3.066920708278495944, -2.499999999999999112 ) ) ;
#5401 = AXIS2_PLACEMENT_3D ( 'NONE', #11830, #12907, #17672 ) ;
#5402 = AXIS2_PLACEMENT_3D ( 'NONE', #12249, #7397, #17998 ) ;
#5403 = CARTESIAN_POINT ( 'NONE',  ( -19.17624791478365864, -18.22898240811121795, 8.660254037844417496 ) ) ;
#5404 = EDGE_CURVE ( 'NONE', #6176, #17712, #16542, .T. ) ;
#5405 = CARTESIAN_POINT ( 'NONE',  ( -65.30644784966793281, -30.60858878180435738, -4.330127018922181215 ) ) ;
#5406 = DIRECTION ( 'NONE',  ( 0.000000000000000000, 0.000000000000000000, 1.000000000000000000 ) ) ;
#5407 = CYLINDRICAL_SURFACE ( 'NONE', #1466, 1.500000000000001554 ) ;
#5408 = ADVANCED_FACE ( 'NONE', ( #1693 ), #637, .F. ) ;
#5409 = ORIENTED_EDGE ( 'NONE', *, *, #14957, .F. ) ;
#5410 = DIRECTION ( 'NONE',  ( -0.1566598588826321192, 0.9876526153536342445, 7.798540720466730171E-17 ) ) ;
#5411 = AXIS2_PLACEMENT_3D ( 'NONE', #13569, #10546, #14912 ) ;
#5412 = VERTEX_POINT ( 'NONE', #5055 ) ;
#5413 = EDGE_LOOP ( 'NONE', ( #18043, #17305, #17956, #12193 ) ) ;
#5414 = DIRECTION ( 'NONE',  ( -0.1566598588826321192, 0.9876526153536342445, 7.798540720466730171E-17 ) ) ;
#5415 = AXIS2_PLACEMENT_3D ( 'NONE', #12498, #6744, #15345 ) ;
#5416 = FACE_BOUND ( 'NONE', #14408, .T. ) ;
#5417 = LINE ( 'NONE', #11178, #7654 ) ;
#5418 = AXIS2_PLACEMENT_3D ( 'NONE', #7411, #14784, #1988 ) ;
#5419 = EDGE_CURVE ( 'NONE', #1622, #18512, #17553, .T. ) ;
#5420 = EDGE_CURVE ( 'NONE', #9991, #15242, #4533, .T. ) ;
#5421 = VECTOR ( 'NONE', #32, 1000.000000000000000 ) ;
#5422 = CARTESIAN_POINT ( 'NONE',  ( -53.90880776292333820, -86.50618184100221697, -8.660254037844385522 ) ) ;
#5423 = EDGE_LOOP ( 'NONE', ( #440, #13 ) ) ;
#5424 = VECTOR ( 'NONE', #15807, 1000.000000000000000 ) ;
#5425 = DIRECTION ( 'NONE',  ( 0.000000000000000000, 1.000000000000000000, 1.914177628664062635E-16 ) ) ;
#5426 = VECTOR ( 'NONE', #14407, 1000.000000000000227 ) ;
#5427 = DIRECTION ( 'NONE',  ( -0.9876526153536336894, -0.1566598588826349503, 0.000000000000000000 ) ) ;
#5429 = ADVANCED_FACE ( 'NONE', ( #10398, #12159 ), #2228, .F. ) ;
#5428 = DIRECTION ( 'NONE',  ( 0.000000000000000000, 0.000000000000000000, 1.000000000000000000 ) ) ;
#5430 = ORIENTED_EDGE ( 'NONE', *, *, #4393, .F. ) ;
#5431 = CARTESIAN_POINT ( 'NONE',  ( 0.000000000000000000, 0.000000000000000000, 30.00000000000000000 ) ) ;
#5432 = DIRECTION ( 'NONE',  ( -0.1566598588826321747, 0.9876526153536343555, 0.000000000000000000 ) ) ;
#5433 = ORIENTED_EDGE ( 'NONE', *, *, #2192, .T. ) ;
#5434 = EDGE_LOOP ( 'NONE', ( #4564, #7316, #37, #2894 ) ) ;
#5435 = CARTESIAN_POINT ( 'NONE',  ( -30.73860631229088369, -25.12549372091224598, -12.99038105676658006 ) ) ;
#5436 = VECTOR ( 'NONE', #6655, 1000.000000000000000 ) ;
#5437 = EDGE_LOOP ( 'NONE', ( #11627, #9516, #11835, #8571 ) ) ;
#5438 = ORIENTED_EDGE ( 'NONE', *, *, #2168, .F. ) ;
#5439 = CARTESIAN_POINT ( 'NONE',  ( 73.09088021254186174, 1.387778780781445676E-14, 110.7545852194966045 ) ) ;
#5440 = EDGE_LOOP ( 'NONE', ( #18127, #8867, #15413, #16755 ) ) ;
#5441 = AXIS2_PLACEMENT_3D ( 'NONE', #722, #13581, #6417 ) ;
#5442 = EDGE_CURVE ( 'NONE', #14934, #17878, #13595, .T. ) ;
#5443 = FACE_OUTER_BOUND ( 'NONE', #12130, .T. ) ;
#5444 = UNCERTAINTY_MEASURE_WITH_UNIT (LENGTH_MEASURE( 1.000000000000000082E-05 ), #4502, 'distance_accuracy_value', 'NONE');
#5445 = CARTESIAN_POINT ( 'NONE',  ( -42.55080268635656893, -84.70459346385194976, 17.32050807568881368 ) ) ;
#5446 = EDGE_CURVE ( 'NONE', #2096, #959, #15988, .T. ) ;
#5447 = AXIS2_PLACEMENT_3D ( 'NONE', #4096, #8485, #1295 ) ;
#5448 = EDGE_CURVE ( 'NONE', #697, #17456, #2104, .T. ) ;
#5449 = EDGE_CURVE ( 'NONE', #5280, #10517, #18464, .T. ) ;
#5450 = DIRECTION ( 'NONE',  ( -1.000000000000000000, -6.938893903907222067E-15, 0.000000000000000000 ) ) ;
#5452 = DIRECTION ( 'NONE',  ( 0.000000000000000000, 0.000000000000000000, 1.000000000000000000 ) ) ;
#5451 = AXIS2_PLACEMENT_3D ( 'NONE', #15474, #16819, #3702 ) ;
#5453 = ORIENTED_EDGE ( 'NONE', *, *, #4909, .F. ) ;
#5455 = ADVANCED_FACE ( 'NONE', ( #266 ), #6509, .F. ) ;
#5454 = CARTESIAN_POINT ( 'NONE',  ( -6.047290928450125946, -21.20899724884646531, -12.99038105676658006 ) ) ;
#5456 = CARTESIAN_POINT ( 'NONE',  ( -9.299721761247353058, -16.66238381928489787, 1.561251128379126385E-14 ) ) ;
#5457 = ORIENTED_EDGE ( 'NONE', *, *, #7206, .T. ) ;
#5458 = ORIENTED_EDGE ( 'NONE', *, *, #8356, .T. ) ;
#5459 = FACE_BOUND ( 'NONE', #17099, .T. ) ;
#5460 = CARTESIAN_POINT ( 'NONE',  ( -45.34904222165485521, -22.38046866850096350, 17.32050807568881723 ) ) ;
#5461 = EDGE_CURVE ( 'NONE', #11609, #2300, #18197, .T. ) ;
#5462 = ORIENTED_EDGE ( 'NONE', *, *, #4446, .F. ) ;
#5463 = CIRCLE ( 'NONE', #16981, 1.500000000000001332 ) ;
#5464 = EDGE_CURVE ( 'NONE', #8283, #15653, #7272, .T. ) ;
#5465 = VERTEX_POINT ( 'NONE', #16845 ) ;
#5466 = ORIENTED_EDGE ( 'NONE', *, *, #4092, .F. ) ;
#5467 = ORIENTED_EDGE ( 'NONE', *, *, #9509, .F. ) ;
#5468 = CYLINDRICAL_SURFACE ( 'NONE', #16080, 1.500000000000001554 ) ;
#5469 = CIRCLE ( 'NONE', #15141, 1.500000000000000888 ) ;
#5470 = AXIS2_PLACEMENT_3D ( 'NONE', #11466, #17300, #1180 ) ;
#5471 = DIRECTION ( 'NONE',  ( -0.9876526153536341335, -0.1566598588826327021, 0.000000000000000000 ) ) ;
#5472 = EDGE_LOOP ( 'NONE', ( #17940, #13218 ) ) ;
#5473 = CIRCLE ( 'NONE', #7888, 2.000000000000000000 ) ;
#5474 = DIRECTION ( 'NONE',  ( -0.9876526153536336894, -0.1566598588826350336, 0.000000000000000000 ) ) ;
#5475 = CYLINDRICAL_SURFACE ( 'NONE', #18287, 139.0000000000000000 ) ;
#5476 = AXIS2_PLACEMENT_3D ( 'NONE', #14427, #15937, #3664 ) ;
#5477 = LINE ( 'NONE', #9750, #15813 ) ;
#5478 = EDGE_CURVE ( 'NONE', #8055, #6192, #9688, .T. ) ;
#5479 = CARTESIAN_POINT ( 'NONE',  ( -27.28182215855319015, -24.57718421482303484, -12.99038105676658006 ) ) ;
#5480 = VERTEX_POINT ( 'NONE', #2416 ) ;
#5481 = CARTESIAN_POINT ( 'NONE',  ( -51.27495791377661760, -23.32042782179675555, 21.65063509461102242 ) ) ;
#5482 = AXIS2_PLACEMENT_3D ( 'NONE', #16959, #15513, #9823 ) ;
#5483 = DIRECTION ( 'NONE',  ( -0.1566598588826321747, 0.9876526153536343555, 0.000000000000000000 ) ) ;
#5484 = DIRECTION ( 'NONE',  ( 1.000000000000000000, 0.000000000000000000, 0.000000000000000000 ) ) ;
#5485 = VERTEX_POINT ( 'NONE', #18671 ) ;
#5486 = EDGE_CURVE ( 'NONE', #9818, #10692, #17531, .T. ) ;
#5487 = DIRECTION ( 'NONE',  ( 2.671473304378624222E-16, 0.000000000000000000, 1.000000000000000000 ) ) ;
#5488 = EDGE_CURVE ( 'NONE', #11204, #8447, #3559, .T. ) ;
#5489 = VERTEX_POINT ( 'NONE', #5552 ) ;
#5490 = EDGE_CURVE ( 'NONE', #16695, #403, #1183, .T. ) ;
#5491 = ORIENTED_EDGE ( 'NONE', *, *, #17021, .T. ) ;
#5492 = CYLINDRICAL_SURFACE ( 'NONE', #11779, 145.0000000000000000 ) ;
#5493 = DIRECTION ( 'NONE',  ( -0.1566598588826321192, 0.9876526153536342445, 7.798540720466730171E-17 ) ) ;
#5494 = ORIENTED_EDGE ( 'NONE', *, *, #2090, .T. ) ;
#5495 = ORIENTED_EDGE ( 'NONE', *, *, #17387, .T. ) ;
#5496 = VECTOR ( 'NONE', #3821, 1000.000000000000000 ) ;
#5497 = CARTESIAN_POINT ( 'NONE',  ( -11.76885329963143434, -17.05403346649147878, -4.330127018922180326 ) ) ;
#5498 = CIRCLE ( 'NONE', #10621, 1.500000000000000888 ) ;
#5499 = DIRECTION ( 'NONE',  ( -0.1566598588826321192, 0.9876526153536342445, 7.798540720466731404E-17 ) ) ;
#5500 = LINE ( 'NONE', #9313, #16459 ) ;
#5501 = CARTESIAN_POINT ( 'NONE',  ( -128.7747222983995528, 9.230544287383699142, -4.051035741711870308 ) ) ;
#5502 = DIRECTION ( 'NONE',  ( 1.438274729681541867E-16, 6.252920376642369977E-17, -1.000000000000000000 ) ) ;
#5503 = CARTESIAN_POINT ( 'NONE',  ( -31.52190560670403841, -20.18723064414411539, 4.330127018922218518 ) ) ;
#5504 = CIRCLE ( 'NONE', #14571, 1.500000000000000888 ) ;
#5505 = LINE ( 'NONE', #18715, #15697 ) ;
#5506 = CARTESIAN_POINT ( 'NONE',  ( -58.84707083969148300, -87.28948113541537168, -8.660254037844385522 ) ) ;
#5507 = DIRECTION ( 'NONE',  ( -0.000000000000000000, -0.000000000000000000, -1.000000000000000000 ) ) ;
#5508 = AXIS2_PLACEMENT_3D ( 'NONE', #335, #14730, #3344 ) ;
#5509 = FACE_BOUND ( 'NONE', #3543, .T. ) ;
#5510 = ORIENTED_EDGE ( 'NONE', *, *, #7659, .F. ) ;
#5511 = EDGE_CURVE ( 'NONE', #16387, #15786, #16607, .T. ) ;
#5512 = CIRCLE ( 'NONE', #3968, 1.499999999999999556 ) ;
#5513 = VERTEX_POINT ( 'NONE', #1301 ) ;
#5514 = ORIENTED_EDGE ( 'NONE', *, *, #8935, .F. ) ;
#5515 = DIRECTION ( 'NONE',  ( -0.1566598588826321747, 0.9876526153536343555, 0.000000000000000000 ) ) ;
#5516 = EDGE_LOOP ( 'NONE', ( #14133, #3059 ) ) ;
#5517 = ORIENTED_EDGE ( 'NONE', *, *, #9371, .F. ) ;
#5518 = DIRECTION ( 'NONE',  ( 1.000000000000000000, 0.000000000000000000, 0.000000000000000000 ) ) ;
#5519 = AXIS2_PLACEMENT_3D ( 'NONE', #6742, #1065, #18436 ) ;
#5520 = EDGE_CURVE ( 'NONE', #8134, #4611, #12625, .T. ) ;
#5521 = FACE_OUTER_BOUND ( 'NONE', #269, .T. ) ;
#5522 = VECTOR ( 'NONE', #11821, 1000.000000000000000 ) ;
#5523 = CYLINDRICAL_SURFACE ( 'NONE', #9164, 1.500000000000000666 ) ;
#5524 = ORIENTED_EDGE ( 'NONE', *, *, #16557, .F. ) ;
#5525 = VECTOR ( 'NONE', #10516, 1000.000000000000000 ) ;
#5526 = DIRECTION ( 'NONE',  ( -0.1566598588826321192, 0.9876526153536342445, 7.798540720466730171E-17 ) ) ;
#5527 = CARTESIAN_POINT ( 'NONE',  ( -73.49714175923330117, -26.84527464665596241, 8.660254037844417496 ) ) ;
#5528 = AXIS2_PLACEMENT_3D ( 'NONE', #942, #3935, #6723 ) ;
#5529 = CARTESIAN_POINT ( 'NONE',  ( -29.21749237908258223, -82.58968536893641499, -8.660254037844385522 ) ) ;
#5530 = CARTESIAN_POINT ( 'NONE',  ( -90.00000000000000000, 34.99999999999999289, 35.00000000000000000 ) ) ;
#5531 = CARTESIAN_POINT ( 'NONE',  ( -14.23798483801550674, -17.44568311369805969, 17.32050807568881368 ) ) ;
#5532 = CARTESIAN_POINT ( 'NONE',  ( -35.47251606811855851, -20.81387007967464342, 8.660254037844417496 ) ) ;
#5533 = VERTEX_POINT ( 'NONE', #15295 ) ;
#5534 = ORIENTED_EDGE ( 'NONE', *, *, #5374, .F. ) ;
#5535 = ORIENTED_EDGE ( 'NONE', *, *, #16977, .T. ) ;
#5536 = ORIENTED_EDGE ( 'NONE', *, *, #1667, .F. ) ;
#5537 = LINE ( 'NONE', #5729, #17015 ) ;
#5538 = ADVANCED_FACE ( 'NONE', ( #15578 ), #1025, .T. ) ;
#5539 = ORIENTED_EDGE ( 'NONE', *, *, #4862, .F. ) ;
#5540 = EDGE_LOOP ( 'NONE', ( #15730, #17261 ) ) ;
#5541 = ORIENTED_EDGE ( 'NONE', *, *, #2244, .T. ) ;
#5542 = DIRECTION ( 'NONE',  ( -0.1566598588826321747, 0.9876526153536343555, 0.000000000000000000 ) ) ;
#5543 = CARTESIAN_POINT ( 'NONE',  ( -20.86208015875458344, -23.55889513208593655, 21.65063509461101177 ) ) ;
#5544 = EDGE_CURVE ( 'NONE', #9534, #9193, #11725, .T. ) ;
#5545 = DIRECTION ( 'NONE',  ( -0.1566598588826321747, 0.9876526153536343555, 0.000000000000000000 ) ) ;
#5546 = DIRECTION ( 'NONE',  ( -1.000000000000000000, 0.000000000000000000, 0.000000000000000000 ) ) ;
#5547 = DIRECTION ( 'NONE',  ( -0.9876526153536336894, -0.1566598588826349503, 0.000000000000000000 ) ) ;
#5548 = ITEM_DEFINED_TRANSFORMATION ( 'NONE', 'NONE', #1742,  #18772 ) ;
#5549 = DIRECTION ( 'NONE',  ( -0.1566598588826321192, 0.9876526153536342445, 7.798540720466730171E-17 ) ) ;
#5550 = DIRECTION ( 'NONE',  ( -1.000000000000000000, 0.000000000000000000, 0.000000000000000000 ) ) ;
#5551 = CARTESIAN_POINT ( 'NONE',  ( -77.65210554158829837, -32.56683701783724416, 8.660254037844417496 ) ) ;
#5552 = CARTESIAN_POINT ( 'NONE',  ( -89.99999999999998579, -35.00000000000001421, -2.499999999999974243 ) ) ;
#5553 = CARTESIAN_POINT ( 'NONE',  ( -61.15148406731293562, -24.88702641062305787, -12.99038105676658006 ) ) ;
#5554 = ORIENTED_EDGE ( 'NONE', *, *, #1958, .F. ) ;
#5555 = ORIENTED_EDGE ( 'NONE', *, *, #4886, .F. ) ;
#5556 = AXIS2_PLACEMENT_3D ( 'NONE', #6929, #3854, #14015 ) ;
#5557 = FACE_BOUND ( 'NONE', #12558, .T. ) ;
#5558 = CARTESIAN_POINT ( 'NONE',  ( -16.87183468716221313, -80.63143713290352821, 4.330127018922213189 ) ) ;
#5559 = ORIENTED_EDGE ( 'NONE', *, *, #14159, .F. ) ;
#5560 = DIRECTION ( 'NONE',  ( -0.9876526153536336894, -0.1566598588826349503, 0.000000000000000000 ) ) ;
#5561 = DIRECTION ( 'NONE',  ( -0.000000000000000000, -0.000000000000000000, -1.000000000000000000 ) ) ;
#5562 = ORIENTED_EDGE ( 'NONE', *, *, #13982, .T. ) ;
#5563 = FACE_OUTER_BOUND ( 'NONE', #7858, .T. ) ;
#5564 = ADVANCED_FACE ( 'NONE', ( #8383 ), #12456, .F. ) ;
#5565 = ADVANCED_FACE ( 'NONE', ( #12731 ), #5265, .F. ) ;
#5566 = LINE ( 'NONE', #11315, #2133 ) ;
#5567 = EDGE_CURVE ( 'NONE', #11377, #6476, #2976, .T. ) ;
#5568 = ORIENTED_EDGE ( 'NONE', *, *, #15232, .F. ) ;
#5569 = CARTESIAN_POINT ( 'NONE',  ( -127.5081579206796221, 9.551524140464916712, 2.822349119005437501 ) ) ;
#5570 = AXIS2_PLACEMENT_3D ( 'NONE', #18529, #17077, #9846 ) ;
#5571 = DIRECTION ( 'NONE',  ( -0.1566598588826321192, 0.9876526153536342445, 7.798540720466730171E-17 ) ) ;
#5572 = DIRECTION ( 'NONE',  ( -0.1566598588826321192, 0.9876526153536342445, 7.798540720466731404E-17 ) ) ;
#5573 = CARTESIAN_POINT ( 'NONE',  ( -47.81817376003893827, -22.77211831570753375, -4.330127018922180326 ) ) ;
#5574 = ORIENTED_EDGE ( 'NONE', *, *, #14426, .T. ) ;
#5575 = CARTESIAN_POINT ( 'NONE',  ( -72.01566283620284992, -26.61028485833201174, -8.660254037844380193 ) ) ;
#5576 = ORIENTED_EDGE ( 'NONE', *, *, #2494, .T. ) ;
#5577 = CARTESIAN_POINT ( 'NONE',  ( -77.65210554158829837, -32.56683701783724416, -17.32050807568878170 ) ) ;
#5578 = CARTESIAN_POINT ( 'NONE',  ( -14.23798483801550674, -17.44568311369805969, 17.32050807568881368 ) ) ;
#5579 = EDGE_LOOP ( 'NONE', ( #6921, #11878, #1053, #3566 ) ) ;
#5580 = CARTESIAN_POINT ( 'NONE',  ( -79.78608161301387725, 31.42857711355109274, 35.00001200000000523 ) ) ;
#5582 = ORIENTED_EDGE ( 'NONE', *, *, #5264, .F. ) ;
#5581 = DIRECTION ( 'NONE',  ( -0.1566598588826321192, 0.9876526153536342445, 7.798540720466730171E-17 ) ) ;
#5583 = ADVANCED_FACE ( 'NONE', ( #5642 ), #16752, .F. ) ;
#5584 = DIRECTION ( 'NONE',  ( -0.9876526153536336894, -0.1566598588826349503, 0.000000000000000000 ) ) ;
#5585 = FACE_OUTER_BOUND ( 'NONE', #4606, .T. ) ;
#5586 = EDGE_LOOP ( 'NONE', ( #83, #9291 ) ) ;
#5587 = ORIENTED_EDGE ( 'NONE', *, *, #6746, .F. ) ;
#5588 = EDGE_CURVE ( 'NONE', #10247, #1314, #11438, .T. ) ;
#5589 = EDGE_CURVE ( 'NONE', #1314, #2452, #10357, .T. ) ;
#5590 = LINE ( 'NONE', #5786, #14577 ) ;
#5591 = CARTESIAN_POINT ( 'NONE',  ( -29.75095369693726610, -24.96883386202961574, -8.660254037844380193 ) ) ;
#5592 = DIRECTION ( 'NONE',  ( -0.1566598588826321192, 0.9876526153536342445, 7.798540720466731404E-17 ) ) ;
#5593 = DIRECTION ( 'NONE',  ( -0.1566598588826321192, 0.9876526153536342445, 7.798540720466730171E-17 ) ) ;
#5594 = DIRECTION ( 'NONE',  ( 3.208277787129350839E-17, 0.000000000000000000, -1.000000000000000000 ) ) ;
#5595 = EDGE_CURVE ( 'NONE', #10837, #3705, #575, .T. ) ;
#5596 = CARTESIAN_POINT ( 'NONE',  ( -5.000000000000004441, 0.000000000000000000, -20.00000000000000355 ) ) ;
#5597 = DIRECTION ( 'NONE',  ( -0.9876526153536341335, -0.1566598588826327021, 0.000000000000000000 ) ) ;
#5598 = DIRECTION ( 'NONE',  ( -0.1566598588826321192, 0.9876526153536342445, 7.798540720466730171E-17 ) ) ;
#5599 = FACE_BOUND ( 'NONE', #2534, .T. ) ;
#5600 = DIRECTION ( 'NONE',  ( 0.000000000000000000, 0.000000000000000000, 1.000000000000000000 ) ) ;
#5601 = DIRECTION ( 'NONE',  ( 0.000000000000000000, 0.000000000000000000, 1.000000000000000000 ) ) ;
#5602 = LINE ( 'NONE', #2839, #14461 ) ;
#5604 = ORIENTED_EDGE ( 'NONE', *, *, #13083, .F. ) ;
#5603 = LINE ( 'NONE', #17173, #14510 ) ;
#5605 = DIRECTION ( 'NONE',  ( -0.9876526153536336894, -0.1566598588826349503, 0.000000000000000000 ) ) ;
#5606 = ORIENTED_EDGE ( 'NONE', *, *, #15024, .T. ) ;
#5607 = ORIENTED_EDGE ( 'NONE', *, *, #2282, .F. ) ;
#5608 = VERTEX_POINT ( 'NONE', #8939 ) ;
#5609 = FACE_OUTER_BOUND ( 'NONE', #3726, .T. ) ;
#5610 = FACE_BOUND ( 'NONE', #10738, .T. ) ;
#5611 = CARTESIAN_POINT ( 'NONE',  ( -31.52190560670403841, -20.18723064414410828, -21.65063509461097979 ) ) ;
#5612 = AXIS2_PLACEMENT_3D ( 'NONE', #1026, #15500, #12539 ) ;
#5613 = VERTEX_POINT ( 'NONE', #14717 ) ;
#5614 = EDGE_CURVE ( 'NONE', #4142, #9088, #15390, .T. ) ;
#5615 = EDGE_CURVE ( 'NONE', #3175, #1556, #263, .T. ) ;
#5616 = DIRECTION ( 'NONE',  ( -0.000000000000000000, -0.000000000000000000, -1.000000000000000000 ) ) ;
#5617 = FACE_BOUND ( 'NONE', #2292, .T. ) ;
#5618 = ORIENTED_EDGE ( 'NONE', *, *, #14968, .T. ) ;
#5619 = DIRECTION ( 'NONE',  ( -0.1566598588826321192, 0.9876526153536342445, 7.798540720466730171E-17 ) ) ;
#5620 = EDGE_CURVE ( 'NONE', #10500, #17370, #6303, .T. ) ;
#5621 = LINE ( 'NONE', #12809, #11196 ) ;
#5622 = CARTESIAN_POINT ( 'NONE',  ( -26.74836084069850983, -82.19803572172985184, 12.99038105676661203 ) ) ;
#5623 = FACE_BOUND ( 'NONE', #16632, .T. ) ;
#5624 = DIRECTION ( 'NONE',  ( -0.9868632313631133801, 0.1615579233078772714, 2.699728182682517290E-16 ) ) ;
#5625 = AXIS2_PLACEMENT_3D ( 'NONE', #2802, #11663, #8940 ) ;
#5626 = ORIENTED_EDGE ( 'NONE', *, *, #9038, .F. ) ;
#5627 = ORIENTED_EDGE ( 'NONE', *, *, #10296, .F. ) ;
#5628 = ORIENTED_EDGE ( 'NONE', *, *, #8606, .F. ) ;
#5629 = CARTESIAN_POINT ( 'NONE',  ( -65.30644784966791860, -30.60858878180435028, 21.65063509461101887 ) ) ;
#5630 = ORIENTED_EDGE ( 'NONE', *, *, #10300, .F. ) ;
#5631 = FACE_BOUND ( 'NONE', #4240, .T. ) ;
#5632 = B_SPLINE_CURVE_WITH_KNOTS ( 'NONE', 3,
 ( #2305, #16841, #6696, #14157, #3900, #5354, #2408, #12244, #18290, #2508, #9805, #12338, #14057, #16933, #8297, #11011, #5165, #2595, #15573, #1103 ),
 .UNSPECIFIED., .F., .F.,
 ( 4, 2, 2, 2, 2, 2, 2, 2, 2, 4 ),
 ( 4.336808689942017736E-19, 0.0009785997360078372773, 0.001467899604011736617, 0.001957199472015635957, 0.002935799208023399508, 0.003914398944031161759, 0.004892998680038927045, 0.005871598416046690597, 0.006850198152054454148, 0.007828797888062217700 ),
 .UNSPECIFIED. ) ;
#5633 = DIRECTION ( 'NONE',  ( -0.9876526153536341335, -0.1566598588826327021, 0.000000000000000000 ) ) ;
#5634 = AXIS2_PLACEMENT_3D ( 'NONE', #2753, #5799, #5601 ) ;
#5635 = DIRECTION ( 'NONE',  ( -0.9876526153536336894, -0.1566598588826349503, 0.000000000000000000 ) ) ;
#5636 = DIRECTION ( 'NONE',  ( -0.1566598588826321192, 0.9876526153536342445, 7.798540720466731404E-17 ) ) ;
#5637 = CYLINDRICAL_SURFACE ( 'NONE', #4282, 1.500000000000001554 ) ;
#5638 = ORIENTED_EDGE ( 'NONE', *, *, #18601, .F. ) ;
#5639 = EDGE_CURVE ( 'NONE', #9448, #14533, #13862, .T. ) ;
#5640 = DIRECTION ( 'NONE',  ( -0.1566598588826321192, 0.9876526153536342445, 7.798540720466730171E-17 ) ) ;
#5641 = DIRECTION ( 'NONE',  ( -0.9876526153536341335, -0.1566598588826327021, 0.000000000000000000 ) ) ;
#5642 = FACE_OUTER_BOUND ( 'NONE', #6711, .T. ) ;
#5643 = DIRECTION ( 'NONE',  ( 0.000000000000000000, 0.000000000000000000, 1.000000000000000000 ) ) ;
#5644 = ORIENTED_EDGE ( 'NONE', *, *, #6966, .F. ) ;
#5645 = VERTEX_POINT ( 'NONE', #13660 ) ;
#5646 = DIRECTION ( 'NONE',  ( -0.000000000000000000, -0.000000000000000000, -1.000000000000000000 ) ) ;
#5647 = EDGE_LOOP ( 'NONE', ( #15476, #15282, #5245, #9861 ) ) ;
#5648 = AXIS2_PLACEMENT_3D ( 'NONE', #1078, #8166, #18450 ) ;
#5649 = ADVANCED_FACE ( 'NONE', ( #614 ), #702, .F. ) ;
#5650 = CARTESIAN_POINT ( 'NONE',  ( -18.39294862037050393, -23.16724548487935564, 8.660254037844417496 ) ) ;
#5651 = CIRCLE ( 'NONE', #10170, 150.0000000000000284 ) ;
#5652 = ORIENTED_EDGE ( 'NONE', *, *, #3676, .F. ) ;
#5653 = DIRECTION ( 'NONE',  ( -0.000000000000000000, -0.000000000000000000, -1.000000000000000000 ) ) ;
#5654 = CARTESIAN_POINT ( 'NONE',  ( -68.55887868246516348, -26.06197535224280060, 1.908195823574487804E-14 ) ) ;
#5655 = VERTEX_POINT ( 'NONE', #4854 ) ;
#5656 = CARTESIAN_POINT ( 'NONE',  ( -2.057045456857760524, -78.28153924966404986, -12.99038105676658539 ) ) ;
#5657 = CIRCLE ( 'NONE', #8062, 1.500000000000000888 ) ;
#5658 = CARTESIAN_POINT ( 'NONE',  ( -23.29157668696081629, -81.64972621564064070, 4.330127018922213189 ) ) ;
#5659 = DIRECTION ( 'NONE',  ( -0.9876526153536344665, -0.1566598588826304539, 0.000000000000000000 ) ) ;
#5660 = EDGE_LOOP ( 'NONE', ( #14979, #3913, #3517, #4634 ) ) ;
#5661 = EDGE_CURVE ( 'NONE', #18619, #14180, #7522, .T. ) ;
#5662 = CARTESIAN_POINT ( 'NONE',  ( -13.45468554360235203, -22.38394619046619383, -8.660254037844380193 ) ) ;
#5663 = AXIS2_PLACEMENT_3D ( 'NONE', #244, #6422, #12058 ) ;
#5664 = ORIENTED_EDGE ( 'NONE', *, *, #15944, .F. ) ;
#5665 = DIRECTION ( 'NONE',  ( -0.1566598588826321192, 0.9876526153536342445, 7.798540720466730171E-17 ) ) ;
#5666 = ORIENTED_EDGE ( 'NONE', *, *, #17995, .F. ) ;
#5667 = CARTESIAN_POINT ( 'NONE',  ( -79.48148684286209686, 1.792690752935663046, 3.092063782402497907 ) ) ;
#5668 = CARTESIAN_POINT ( 'NONE',  ( -50.45202360918564466, -85.95787233491300583, 1.424741226644455312E-14 ) ) ;
#5669 = ORIENTED_EDGE ( 'NONE', *, *, #4965, .T. ) ;
#5670 = EDGE_LOOP ( 'NONE', ( #9242, #10762, #3445, #9129, #3947, #6361, #7881, #3095, #8995, #9799, #5728 ) ) ;
#5671 = CARTESIAN_POINT ( 'NONE',  ( -11.93357161039406300, -79.84813783849037350, -4.330127018922185655 ) ) ;
#5672 = DIRECTION ( 'NONE',  ( 0.000000000000000000, 0.000000000000000000, 1.000000000000000000 ) ) ;
#5673 = ORIENTED_EDGE ( 'NONE', *, *, #9562, .F. ) ;
#5674 = ADVANCED_FACE ( 'NONE', ( #16238 ), #11859, .F. ) ;
#5675 = AXIS2_PLACEMENT_3D ( 'NONE', #9549, #15427, #948 ) ;
#5676 = CIRCLE ( 'NONE', #4745, 1.500000000000000444 ) ;
#5677 = CYLINDRICAL_SURFACE ( 'NONE', #3283, 1.500000000000001554 ) ;
#5678 = VERTEX_POINT ( 'NONE', #4761 ) ;
#5679 = EDGE_LOOP ( 'NONE', ( #9118, #8715, #10420, #3255 ) ) ;
#5680 = CIRCLE ( 'NONE', #7207, 1.500000000000001332 ) ;
#5681 = DIRECTION ( 'NONE',  ( -0.1566598588826321192, 0.9876526153536342445, 7.798540720466730171E-17 ) ) ;
#5682 = CIRCLE ( 'NONE', #16263, 1.500000000000001332 ) ;
#5683 = ORIENTED_EDGE ( 'NONE', *, *, #169, .T. ) ;
#5684 = DIRECTION ( 'NONE',  ( 0.000000000000000000, 0.000000000000000000, -1.000000000000000000 ) ) ;
#5685 = CARTESIAN_POINT ( 'NONE',  ( -62.63296299034339398, -25.12201619894701210, 4.330127018922218518 ) ) ;
#5686 = EDGE_CURVE ( 'NONE', #7926, #4290, #8132, .T. ) ;
#5687 = DIRECTION ( 'NONE',  ( -0.1566598588826321192, 0.9876526153536342445, 7.798540720466730171E-17 ) ) ;
#5688 = CARTESIAN_POINT ( 'NONE',  ( -61.31620237807555895, -87.68113078262194904, 4.330127018922213189 ) ) ;
#5689 = VECTOR ( 'NONE', #1838, 1000.000000000000000 ) ;
#5690 = DIRECTION ( 'NONE',  ( -0.1566598588826321192, 0.9876526153536342445, 7.798540720466730171E-17 ) ) ;
#5691 = CYLINDRICAL_SURFACE ( 'NONE', #790, 1.500000000000001554 ) ;
#5692 = EDGE_CURVE ( 'NONE', #17705, #12460, #5101, .T. ) ;
#5693 = ADVANCED_FACE ( 'NONE', ( #14812, #6402 ), #421, .F. ) ;
#5694 = DIRECTION ( 'NONE',  ( -1.000000000000000000, 0.000000000000000000, 0.000000000000000000 ) ) ;
#5695 = ADVANCED_FACE ( 'NONE', ( #3332 ), #9136, .T. ) ;
#5696 = ORIENTED_EDGE ( 'NONE', *, *, #10214, .F. ) ;
#5697 = VECTOR ( 'NONE', #14045, 1000.000000000000000 ) ;
#5698 = EDGE_CURVE ( 'NONE', #5366, #2319, #10839, .T. ) ;
#5699 = ORIENTED_EDGE ( 'NONE', *, *, #17207, .F. ) ;
#5700 = ORIENTED_EDGE ( 'NONE', *, *, #18466, .F. ) ;
#5701 = CYLINDRICAL_SURFACE ( 'NONE', #16631, 1.500000000000001554 ) ;
#5702 = ORIENTED_EDGE ( 'NONE', *, *, #13651, .T. ) ;
#5703 = ORIENTED_EDGE ( 'NONE', *, *, #8346, .F. ) ;
#5704 = CARTESIAN_POINT ( 'NONE',  ( -79.05438463828195950, 1.499069270643396345, -3.389939594122236333 ) ) ;
#5705 = CIRCLE ( 'NONE', #10174, 1.500000000000000888 ) ;
#5706 = ORIENTED_EDGE ( 'NONE', *, *, #118, .F. ) ;
#5707 = DIRECTION ( 'NONE',  ( -0.1566598588826321747, 0.9876526153536343555, 0.000000000000000000 ) ) ;
#5708 = DIRECTION ( 'NONE',  ( -0.1566598588826321192, 0.9876526153536342445, 7.798540720466730171E-17 ) ) ;
#5709 = AXIS2_PLACEMENT_3D ( 'NONE', #8683, #15976, #7280 ) ;
#5710 = DIRECTION ( 'NONE',  ( -0.1566598588826321747, 0.9876526153536343555, 0.000000000000000000 ) ) ;
#5711 = VERTEX_POINT ( 'NONE', #9307 ) ;
#5712 = LINE ( 'NONE', #4279, #5094 ) ;
#5713 = ORIENTED_EDGE ( 'NONE', *, *, #3267, .T. ) ;
#5714 = EDGE_CURVE ( 'NONE', #1641, #14006, #895, .T. ) ;
#5715 = DIRECTION ( 'NONE',  ( -0.9876526153536336894, -0.1566598588826349503, 0.000000000000000000 ) ) ;
#5716 = DIRECTION ( 'NONE',  ( -0.9876526153536341335, -0.1566598588826327021, 0.000000000000000000 ) ) ;
#5717 = AXIS2_PLACEMENT_3D ( 'NONE', #11863, #10452, #4860 ) ;
#5718 = DIRECTION ( 'NONE',  ( 1.438274729681541867E-16, 6.252920376642369977E-17, -1.000000000000000000 ) ) ;
#5719 = AXIS2_PLACEMENT_3D ( 'NONE', #7080, #12725, #4303 ) ;
#5720 = ORIENTED_EDGE ( 'NONE', *, *, #174, .F. ) ;
#5721 = CARTESIAN_POINT ( 'NONE',  ( -41.60278508118079799, -26.84875216862118918, 8.660254037844417496 ) ) ;
#5722 = VERTEX_POINT ( 'NONE', #18561 ) ;
#5723 = AXIS2_PLACEMENT_3D ( 'NONE', #3422, #6487, #13744 ) ;
#5724 = ORIENTED_EDGE ( 'NONE', *, *, #5377, .F. ) ;
#5725 = EDGE_CURVE ( 'NONE', #5005, #8991, #6677, .T. ) ;
#5726 = STYLED_ITEM ( 'NONE', ( #16963 ), #10448 ) ;
#5727 = VERTEX_POINT ( 'NONE', #12704 ) ;
#5728 = ORIENTED_EDGE ( 'NONE', *, *, #7403, .T. ) ;
#5729 = CARTESIAN_POINT ( 'NONE',  ( -110.7369027592740167, -34.07064978273316314, 2.500000000000000000 ) ) ;
#5730 = ORIENTED_EDGE ( 'NONE', *, *, #9435, .T. ) ;
#5731 = CYLINDRICAL_SURFACE ( 'NONE', #13063, 1.500000000000000666 ) ;
#5732 = AXIS2_PLACEMENT_3D ( 'NONE', #4917, #16495, #4825 ) ;
#5733 = AXIS2_PLACEMENT_3D ( 'NONE', #15760, #4076, #7240 ) ;
#5734 = LINE ( 'NONE', #14155, #9111 ) ;
#5735 = VECTOR ( 'NONE', #3182, 1000.000000000000114 ) ;
#5736 = CIRCLE ( 'NONE', #13282, 1.499999999999999556 ) ;
#5737 = DIRECTION ( 'NONE',  ( -0.9710487832595061652, 0.2388812686885108949, 1.369518533665900065E-16 ) ) ;
#5738 = ORIENTED_EDGE ( 'NONE', *, *, #4127, .F. ) ;
#5739 = CARTESIAN_POINT ( 'NONE',  ( -172.4977872642596424, 56.55098501587584536, 2.500000000000000000 ) ) ;
#5740 = CYLINDRICAL_SURFACE ( 'NONE', #13821, 1.500000000000001554 ) ;
#5741 = DIRECTION ( 'NONE',  ( -0.000000000000000000, -0.000000000000000000, -1.000000000000000000 ) ) ;
#5742 = VECTOR ( 'NONE', #6977, 1000.000000000000000 ) ;
#5743 = DIRECTION ( 'NONE',  ( -0.1566598588826321192, 0.9876526153536342445, 7.798540720466730171E-17 ) ) ;
#5744 = EDGE_LOOP ( 'NONE', ( #13268, #16049, #7515, #7025 ) ) ;
#5745 = ORIENTED_EDGE ( 'NONE', *, *, #6326, .T. ) ;
#5746 = FACE_OUTER_BOUND ( 'NONE', #12068, .T. ) ;
#5747 = ORIENTED_EDGE ( 'NONE', *, *, #18025, .T. ) ;
#5748 = CIRCLE ( 'NONE', #16027, 1.500000000000001332 ) ;
#5749 = EDGE_CURVE ( 'NONE', #11814, #10450, #11736, .T. ) ;
#5750 = CARTESIAN_POINT ( 'NONE',  ( 2.447859171744379392, -14.79900155049412369, 24.99999999999998934 ) ) ;
#5751 = ORIENTED_EDGE ( 'NONE', *, *, #7442, .T. ) ;
#5752 = CIRCLE ( 'NONE', #16329, 1.500000000000000888 ) ;
#5753 = DIRECTION ( 'NONE',  ( 0.000000000000000000, 0.000000000000000000, 1.000000000000000000 ) ) ;
#5754 = CARTESIAN_POINT ( 'NONE',  ( -176.1167811578620501, -139.6880237571007513, -2.500000000000000000 ) ) ;
#5755 = AXIS2_PLACEMENT_3D ( 'NONE', #1943, #3160, #17711 ) ;
#5756 = AXIS2_PLACEMENT_3D ( 'NONE', #10829, #16652, #3631 ) ;
#5757 = CIRCLE ( 'NONE', #14226, 1.499999999999999556 ) ;
#5758 = ORIENTED_EDGE ( 'NONE', *, *, #7293, .T. ) ;
#5759 = DIRECTION ( 'NONE',  ( -0.9876526153536341335, -0.1566598588826327021, 0.000000000000000000 ) ) ;
#5760 = EDGE_CURVE ( 'NONE', #13736, #10706, #6965, .T. ) ;
#5761 = FACE_OUTER_BOUND ( 'NONE', #10254, .T. ) ;
#5762 = AXIS2_PLACEMENT_3D ( 'NONE', #18304, #8649, #18737 ) ;
#5764 = CARTESIAN_POINT ( 'NONE',  ( -128.5664531142841440, 9.331354376930727668, 3.724467847532855647 ) ) ;
#5763 = AXIS2_PLACEMENT_3D ( 'NONE', #5654, #14712, #4020 ) ;
#5765 = AXIS2_PLACEMENT_3D ( 'NONE', #10444, #1836, #1925 ) ;
#5766 = DIRECTION ( 'NONE',  ( -1.224646799147353207E-16, 1.000000000000000000, 0.000000000000000000 ) ) ;
#5767 = DIRECTION ( 'NONE',  ( 0.000000000000000000, 0.000000000000000000, 1.000000000000000000 ) ) ;
#5768 = FILL_AREA_STYLE_COLOUR ( '', #11989 ) ;
#5769 = ORIENTED_EDGE ( 'NONE', *, *, #15359, .T. ) ;
#5770 = AXIS2_PLACEMENT_3D ( 'NONE', #7649, #13482, #4780 ) ;
#5771 = FACE_OUTER_BOUND ( 'NONE', #9245, .T. ) ;
#5772 = AXIS2_PLACEMENT_3D ( 'NONE', #13500, #18311, #9346 ) ;
#5773 = ORIENTED_EDGE ( 'NONE', *, *, #5318, .T. ) ;
#5774 = CARTESIAN_POINT ( 'NONE',  ( -49.79347899074616635, -23.08543803347280843, 12.99038105676661736 ) ) ;
#5775 = CARTESIAN_POINT ( 'NONE',  ( -77.72973689007648090, 30.96463005215034059, -35.00000000000000000 ) ) ;
#5776 = ORIENTED_EDGE ( 'NONE', *, *, #10421, .T. ) ;
#5777 = CARTESIAN_POINT ( 'NONE',  ( 0.000000000000000000, 0.000000000000000000, 30.00000000000000000 ) ) ;
#5778 = ORIENTED_EDGE ( 'NONE', *, *, #11895, .T. ) ;
#5779 = ORIENTED_EDGE ( 'NONE', *, *, #8584, .T. ) ;
#5780 = AXIS2_PLACEMENT_3D ( 'NONE', #15522, #6819, #9836 ) ;
#5781 = VERTEX_POINT ( 'NONE', #18272 ) ;
#5782 = ORIENTED_EDGE ( 'NONE', *, *, #12350, .F. ) ;
#5783 = AXIS2_PLACEMENT_3D ( 'NONE', #3144, #4662, #1834 ) ;
#5784 = EDGE_CURVE ( 'NONE', #13518, #9146, #12319, .T. ) ;
#5785 = AXIS2_PLACEMENT_3D ( 'NONE', #6233, #11963, #14935 ) ;
#5786 = CARTESIAN_POINT ( 'NONE',  ( -1.069392841504132052, -78.12487939078141608, 17.32050807568880657 ) ) ;
#5787 = DIRECTION ( 'NONE',  ( -0.9876526153536336894, -0.1566598588826349503, 0.000000000000000000 ) ) ;
#5788 = DIRECTION ( 'NONE',  ( -0.1566598588826321192, 0.9876526153536342445, 7.798540720466730171E-17 ) ) ;
#5789 = EDGE_LOOP ( 'NONE', ( #13960, #12487, #4887, #18586, #14410, #6827, #5997, #12112, #14473 ) ) ;
#5790 = CARTESIAN_POINT ( 'NONE',  ( -84.23462711737164454, 33.01666666666666572, 30.00000000000000000 ) ) ;
#5791 = CARTESIAN_POINT ( 'NONE',  ( -69.99999999999998579, -45.00000000000000711, 25.00000000000000000 ) ) ;
#5792 = EDGE_CURVE ( 'NONE', #16790, #8885, #12520, .T. ) ;
#5793 = VECTOR ( 'NONE', #151, 1000.000000000000000 ) ;
#5794 = CARTESIAN_POINT ( 'NONE',  ( -2.000000000000000000, 0.000000000000000000, 35.00000000000000000 ) ) ;
#5795 = ORIENTED_EDGE ( 'NONE', *, *, #8193, .F. ) ;
#5796 = CIRCLE ( 'NONE', #13029, 1.500000000000000888 ) ;
#5797 = CARTESIAN_POINT ( 'NONE',  ( -34.15575545585073058, -83.37298466334958391, 8.660254037844412167 ) ) ;
#5798 = CARTESIAN_POINT ( 'NONE',  ( -57.89905323451571206, -29.43363984018462176, -8.660254037844380193 ) ) ;
#5799 = DIRECTION ( 'NONE',  ( -0.1566598588826321192, 0.9876526153536342445, 7.798540720466731404E-17 ) ) ;
#5801 = ORIENTED_EDGE ( 'NONE', *, *, #12727, .T. ) ;
#5800 = DIRECTION ( 'NONE',  ( 1.000000000000000000, -0.000000000000000000, -0.000000000000000000 ) ) ;
#5802 = VERTEX_POINT ( 'NONE', #12430 ) ;
#5803 = CARTESIAN_POINT ( 'NONE',  ( -55.42992169613162190, -29.04199019297804085, 4.330127018922217630 ) ) ;
#5804 = VERTEX_POINT ( 'NONE', #14141 ) ;
#5805 = VERTEX_POINT ( 'NONE', #5138 ) ;
#5806 = AXIS2_PLACEMENT_3D ( 'NONE', #18527, #10114, #5684 ) ;
#5807 = CARTESIAN_POINT ( 'NONE',  ( -74.97862068226375243, -27.08026443497990954, 8.660254037844417496 ) ) ;
#5808 = AXIS2_PLACEMENT_3D ( 'NONE', #9629, #5270, #11023 ) ;
#5809 = FACE_OUTER_BOUND ( 'NONE', #16822, .T. ) ;
#5810 = EDGE_CURVE ( 'NONE', #2328, #5513, #9653, .T. ) ;
#5811 = CIRCLE ( 'NONE', #13953, 139.0000000000000000 ) ;
#5812 = EDGE_CURVE ( 'NONE', #8478, #8527, #3883, .T. ) ;
#5813 = FACE_OUTER_BOUND ( 'NONE', #13152, .T. ) ;
#5814 = EDGE_CURVE ( 'NONE', #11180, #18706, #2373, .T. ) ;
#5815 = AXIS2_PLACEMENT_3D ( 'NONE', #16633, #13671, #6315 ) ;
#5816 = DIRECTION ( 'NONE',  ( -0.5989998693185457634, -0.8007491221077703836, -1.387778780781445429E-16 ) ) ;
#5817 = AXIS2_PLACEMENT_3D ( 'NONE', #10113, #11429, #9765 ) ;
#5818 = CIRCLE ( 'NONE', #7338, 1.500000000000000888 ) ;
#5819 = ORIENTED_EDGE ( 'NONE', *, *, #18681, .F. ) ;
#5820 = DIRECTION ( 'NONE',  ( -0.9876526153536341335, -0.1566598588826327021, 0.000000000000000000 ) ) ;
#5821 = CARTESIAN_POINT ( 'NONE',  ( -2.879979761448749009, -15.64409473654778893, 8.660254037844412167 ) ) ;
#5822 = DIRECTION ( 'NONE',  ( 0.000000000000000000, -0.000000000000000000, -1.000000000000000000 ) ) ;
#5823 = ORIENTED_EDGE ( 'NONE', *, *, #2752, .T. ) ;
#5824 = FACE_BOUND ( 'NONE', #16901, .T. ) ;
#5825 = DIRECTION ( 'NONE',  ( -0.1566598588826321192, 0.9876526153536342445, 7.798540720466731404E-17 ) ) ;
#5826 = ORIENTED_EDGE ( 'NONE', *, *, #7331, .F. ) ;
#5827 = EDGE_LOOP ( 'NONE', ( #2252, #13808, #14091, #6121 ) ) ;
#5828 = VERTEX_POINT ( 'NONE', #2497 ) ;
#5829 = CARTESIAN_POINT ( 'NONE',  ( -90.00000000000001421, 34.99999999999996447, 2.500000000000000000 ) ) ;
#5830 = ORIENTED_EDGE ( 'NONE', *, *, #18468, .F. ) ;
#5831 = FACE_BOUND ( 'NONE', #12792, .T. ) ;
#5832 = CIRCLE ( 'NONE', #16737, 2.999999999999999112 ) ;
#5833 = CARTESIAN_POINT ( 'NONE',  ( -36.62488699423481364, -83.76463431055616127, -12.99038105676658539 ) ) ;
#5834 = EDGE_CURVE ( 'NONE', #12466, #3591, #14195, .T. ) ;
#5835 = VERTEX_POINT ( 'NONE', #2579 ) ;
#5836 = AXIS2_PLACEMENT_3D ( 'NONE', #12554, #16962, #18404 ) ;
#5837 = APPLICATION_PROTOCOL_DEFINITION ( 'draft international standard', 'automotive_design', 1998, #9441 ) ;
#5838 = LINE ( 'NONE', #1383, #4843 ) ;
#5839 = DIRECTION ( 'NONE',  ( -0.1566598588826321192, 0.9876526153536342445, 7.798540720466731404E-17 ) ) ;
#5840 = CARTESIAN_POINT ( 'NONE',  ( -70.94787397664823914, 45.40332465903016868, -4.449065472295569812 ) ) ;
#5841 = ORIENTED_EDGE ( 'NONE', *, *, #12541, .T. ) ;
#5842 = EDGE_LOOP ( 'NONE', ( #9662, #204, #14896, #3324 ) ) ;
#5843 = CARTESIAN_POINT ( 'NONE',  ( -52.96079015774754595, -28.65034054577145994, 17.32050807568881723 ) ) ;
#5844 = CARTESIAN_POINT ( 'NONE',  ( -15.88418207180859021, -80.47477727402089442, 1.424741226644455312E-14 ) ) ;
#5845 = DIRECTION ( 'NONE',  ( 0.000000000000000000, 0.000000000000000000, 1.000000000000000000 ) ) ;
#5846 = CIRCLE ( 'NONE', #10666, 2.000000000000000000 ) ;
#5847 = AXIS2_PLACEMENT_3D ( 'NONE', #11003, #12330, #18176 ) ;
#5848 = EDGE_LOOP ( 'NONE', ( #2668, #5823 ) ) ;
#5849 = FACE_OUTER_BOUND ( 'NONE', #1668, .T. ) ;
#5850 = DIRECTION ( 'NONE',  ( -0.1566598588826321192, 0.9876526153536342445, 7.798540720466731404E-17 ) ) ;
#5851 = DIRECTION ( 'NONE',  ( -1.000000000000000000, -1.224646799147353207E-16, 0.000000000000000000 ) ) ;
#5852 = LINE ( 'NONE', #238, #17871 ) ;
#5853 = SHAPE_REPRESENTATION_RELATIONSHIP ( 'NONE' , 'NONE' ,  #13723, #9123 ) ;
#5854 = ADVANCED_FACE ( 'NONE', ( #9592 ), #15369, .F. ) ;
#5855 = EDGE_CURVE ( 'NONE', #1633, #10598, #2076, .T. ) ;
#5856 = AXIS2_PLACEMENT_3D ( 'NONE', #7328, #15925, #7409 ) ;
#5857 = CARTESIAN_POINT ( 'NONE',  ( 1.360103686702108128, -20.03404830722672259, 17.32050807568881012 ) ) ;
#5858 = CARTESIAN_POINT ( 'NONE',  ( -79.50968810220766159, 31.87664632526870889, -30.00000000000000355 ) ) ;
#5859 = CARTESIAN_POINT ( 'NONE',  ( -3.373806069125576901, -15.72242466598909871, -4.330127018922183879 ) ) ;
#5860 = VERTEX_POINT ( 'NONE', #12606 ) ;
#5861 = FACE_OUTER_BOUND ( 'NONE', #14471, .T. ) ;
#5862 = EDGE_CURVE ( 'NONE', #7429, #898, #13265, .T. ) ;
#5864 = ORIENTED_EDGE ( 'NONE', *, *, #7179, .F. ) ;
#5863 = CARTESIAN_POINT ( 'NONE',  ( -18.39294862037050393, -23.16724548487935564, 17.32050807568881012 ) ) ;
#5865 = EDGE_LOOP ( 'NONE', ( #11447, #12404 ) ) ;
#5866 = CARTESIAN_POINT ( 'NONE',  ( -36.62488699423482785, -83.76463431055616127, -21.65063509461098690 ) ) ;
#5867 = ORIENTED_EDGE ( 'NONE', *, *, #6828, .F. ) ;
#5868 = AXIS2_PLACEMENT_3D ( 'NONE', #836, #15514, #13890 ) ;
#5869 = DIRECTION ( 'NONE',  ( -0.1566598588826321192, 0.9876526153536342445, 7.798540720466730171E-17 ) ) ;
#5870 = CARTESIAN_POINT ( 'NONE',  ( -10.98555400521827607, -21.99229654325962002, 21.65063509461101177 ) ) ;
#5871 = CARTESIAN_POINT ( 'NONE',  ( 9.300959619709004755, -76.47995087251376845, 21.65063509461100821 ) ) ;
#5872 = VERTEX_POINT ( 'NONE', #9791 ) ;
#5873 = DIRECTION ( 'NONE',  ( -0.1566598588826321747, 0.9876526153536343555, 0.000000000000000000 ) ) ;
#5874 = PLANE ( 'NONE',  #15066 ) ;
#5875 = DIRECTION ( 'NONE',  ( -0.1566598588826321747, 0.9876526153536343555, 0.000000000000000000 ) ) ;
#5876 = FACE_OUTER_BOUND ( 'NONE', #2258, .T. ) ;
#5877 = ORIENTED_EDGE ( 'NONE', *, *, #15746, .T. ) ;
#5878 = DIRECTION ( 'NONE',  ( 1.000000000000000000, 0.000000000000000000, 0.000000000000000000 ) ) ;
#5879 = DIRECTION ( 'NONE',  ( 0.9868632313631133801, 0.1615579233078775490, 0.000000000000000000 ) ) ;
#5880 = EDGE_CURVE ( 'NONE', #15891, #2138, #1181, .T. ) ;
#5881 = VERTEX_POINT ( 'NONE', #11060 ) ;
#5882 = ORIENTED_EDGE ( 'NONE', *, *, #16890, .F. ) ;
#5883 = CARTESIAN_POINT ( 'NONE',  ( -73.70149508017377116, -31.94019758230671258, -12.99038105676658006 ) ) ;
#5884 = VERTEX_POINT ( 'NONE', #13602 ) ;
#5885 = EDGE_CURVE ( 'NONE', #17245, #1063, #11144, .T. ) ;
#5886 = VERTEX_POINT ( 'NONE', #2326 ) ;
#5887 = DIRECTION ( 'NONE',  ( -0.000000000000000000, -0.000000000000000000, -1.000000000000000000 ) ) ;
#5888 = FACE_BOUND ( 'NONE', #16738, .T. ) ;
#5889 = VERTEX_POINT ( 'NONE', #10671 ) ;
#5890 = CARTESIAN_POINT ( 'NONE',  ( -77.65210554158829837, -32.56683701783724416, 17.32050807568881723 ) ) ;
#5891 = LINE ( 'NONE', #14607, #11495 ) ;
#5892 = FACE_OUTER_BOUND ( 'NONE', #9347, .T. ) ;
#5893 = VERTEX_POINT ( 'NONE', #9250 ) ;
#5894 = VERTEX_POINT ( 'NONE', #739 ) ;
#5895 = ADVANCED_FACE ( 'NONE', ( #12262 ), #5066, .F. ) ;
#5896 = DIRECTION ( 'NONE',  ( -0.1566598588826321192, 0.9876526153536342445, 7.798540720466731404E-17 ) ) ;
#5897 = CYLINDRICAL_SURFACE ( 'NONE', #6389, 1.500000000000000666 ) ;
#5898 = CARTESIAN_POINT ( 'NONE',  ( -51.43967622453925514, -86.11453219379563961, 21.65063509461101532 ) ) ;
#5899 = DIRECTION ( 'NONE',  ( -0.9876526153536336894, -0.1566598588826349503, 0.000000000000000000 ) ) ;
#5900 = ADVANCED_FACE ( 'NONE', ( #2150 ), #2236, .F. ) ;
#5901 = ORIENTED_EDGE ( 'NONE', *, *, #18359, .T. ) ;
#5902 = EDGE_CURVE ( 'NONE', #17941, #6457, #18730, .T. ) ;
#5903 = ORIENTED_EDGE ( 'NONE', *, *, #10465, .F. ) ;
#5904 = ORIENTED_EDGE ( 'NONE', *, *, #8475, .T. ) ;
#5905 = CARTESIAN_POINT ( 'NONE',  ( -52.75643683680709728, -23.55541761012068847, -12.99038105676658006 ) ) ;
#5906 = ORIENTED_EDGE ( 'NONE', *, *, #11599, .F. ) ;
#5907 = AXIS2_PLACEMENT_3D ( 'NONE', #4122, #8409, #2270 ) ;
#5908 = DIRECTION ( 'NONE',  ( -0.000000000000000000, -0.000000000000000000, 1.000000000000000000 ) ) ;
#5909 = CARTESIAN_POINT ( 'NONE',  ( -15.22563745336913144, -17.60234297258069347, 12.99038105676661381 ) ) ;
#5910 = ORIENTED_EDGE ( 'NONE', *, *, #150, .T. ) ;
#5911 = CARTESIAN_POINT ( 'NONE',  ( -89.99999999999998579, -35.00000000000001421, -30.00000000000000355 ) ) ;
#5912 = DIRECTION ( 'NONE',  ( -0.1566598588826321747, 0.9876526153536343555, 0.000000000000000000 ) ) ;
#5913 = CIRCLE ( 'NONE', #8344, 1.500000000000000888 ) ;
#5914 = DIRECTION ( 'NONE',  ( 0.000000000000000000, 0.000000000000000000, -1.000000000000000000 ) ) ;
#5915 = EDGE_CURVE ( 'NONE', #10816, #8368, #5676, .T. ) ;
#5916 = CARTESIAN_POINT ( 'NONE',  ( -174.6158025762232171, 55.77168144464769028, -4.051035741711864091 ) ) ;
#5917 = CARTESIAN_POINT ( 'NONE',  ( -69.99999999999998579, -45.00000000000000711, 20.00000000000001776 ) ) ;
#5918 = EDGE_CURVE ( 'NONE', #7914, #753, #830, .T. ) ;
#5919 = CARTESIAN_POINT ( 'NONE',  ( -58.84707083969148300, -87.28948113541537168, 17.32050807568881368 ) ) ;
#5920 = ORIENTED_EDGE ( 'NONE', *, *, #1675, .T. ) ;
#5921 = ORIENTED_EDGE ( 'NONE', *, *, #13337, .F. ) ;
#5922 = DIRECTION ( 'NONE',  ( -0.1566598588826321192, 0.9876526153536342445, 7.798540720466730171E-17 ) ) ;
#5923 = EDGE_CURVE ( 'NONE', #5152, #7813, #10490, .T. ) ;
#5924 = ORIENTED_EDGE ( 'NONE', *, *, #13427, .F. ) ;
#5925 = CARTESIAN_POINT ( 'NONE',  ( -21.81009776393036503, -81.41473642731668292, -12.99038105676658539 ) ) ;
#5926 = APPLICATION_CONTEXT ( 'automotive_design' ) ;
#5927 = ORIENTED_EDGE ( 'NONE', *, *, #3668, .T. ) ;
#5928 = CYLINDRICAL_SURFACE ( 'NONE', #7012, 1.500000000000001554 ) ;
#5929 = AXIS2_PLACEMENT_3D ( 'NONE', #9594, #2498, #15370 ) ;
#5930 = FACE_BOUND ( 'NONE', #16575, .T. ) ;
#5931 = CARTESIAN_POINT ( 'NONE',  ( -30.53425299135042081, -20.03057078526147450, -17.32050807568878170 ) ) ;
#5932 = DIRECTION ( 'NONE',  ( -0.9876526153536341335, -0.1566598588826327021, 0.000000000000000000 ) ) ;
#5933 = AXIS2_PLACEMENT_3D ( 'NONE', #5017, #13030, #15552 ) ;
#5934 = DIRECTION ( 'NONE',  ( -0.9876526153536336894, -0.1566598588826349503, 0.000000000000000000 ) ) ;
#5935 = CARTESIAN_POINT ( 'NONE',  ( -52.75643683680706886, -23.55541761012070268, 21.65063509461101887 ) ) ;
#5936 = DIRECTION ( 'NONE',  ( -0.1566598588826321192, 0.9876526153536342445, 7.798540720466730171E-17 ) ) ;
#5937 = ORIENTED_EDGE ( 'NONE', *, *, #15974, .F. ) ;
#5938 = CARTESIAN_POINT ( 'NONE',  ( -54.89646037827696290, -86.66284169988483654, -4.330127018922185655 ) ) ;
#5939 = CIRCLE ( 'NONE', #8949, 12.83663829214476060 ) ;
#5940 = EDGE_LOOP ( 'NONE', ( #3406, #5314, #4407, #10524 ) ) ;
#5941 = EDGE_LOOP ( 'NONE', ( #11044, #1177, #11845, #1125 ) ) ;
#5942 = CARTESIAN_POINT ( 'NONE',  ( -9.997901389864651378, -21.83563668437698269, 1.522258424776792809E-14 ) ) ;
#5943 = LINE ( 'NONE', #17352, #16359 ) ;
#5944 = EDGE_LOOP ( 'NONE', ( #5683, #12415 ) ) ;
#5945 = EDGE_CURVE ( 'NONE', #15653, #8283, #4105, .T. ) ;
#5946 = EDGE_CURVE ( 'NONE', #16090, #13071, #12692, .T. ) ;
#5947 = CIRCLE ( 'NONE', #2299, 1.500000000000000888 ) ;
#5948 = CARTESIAN_POINT ( 'NONE',  ( -24.27922930231443743, -81.80638607452327449, 8.660254037844412167 ) ) ;
#5949 = CARTESIAN_POINT ( 'NONE',  ( -45.01993422474063777, -85.09624311105854133, 21.65063509461101532 ) ) ;
#5950 = DIRECTION ( 'NONE',  ( 0.000000000000000000, 2.168404344971010840E-16, 1.000000000000000000 ) ) ;
#5951 = DIRECTION ( 'NONE',  ( 0.000000000000000000, 0.000000000000000000, 1.000000000000000000 ) ) ;
#5952 = AXIS2_PLACEMENT_3D ( 'NONE', #11509, #10185, #14466 ) ;
#5953 = DIRECTION ( 'NONE',  ( -0.9876526153536336894, -0.1566598588826349503, 0.000000000000000000 ) ) ;
#5954 = DIRECTION ( 'NONE',  ( -0.9876526153536341335, -0.1566598588826327576, 0.000000000000000000 ) ) ;
#5955 = CYLINDRICAL_SURFACE ( 'NONE', #18782, 1.500000000000001554 ) ;
#5956 = ORIENTED_EDGE ( 'NONE', *, *, #14218, .F. ) ;
#5957 = CARTESIAN_POINT ( 'NONE',  ( -76.90911978745816668, 1.387778780781445676E-14, -7.500000000000000000 ) ) ;
#5958 = AXIS2_PLACEMENT_3D ( 'NONE', #3166, #1406, #13129 ) ;
#5959 = PLANE ( 'NONE',  #12012 ) ;
#5960 = DIRECTION ( 'NONE',  ( 0.8007491221077702725, -0.5989998693185459855, -1.826024711554533667E-16 ) ) ;
#5961 = AXIS2_PLACEMENT_3D ( 'NONE', #17000, #1169, #6949 ) ;
#5962 = ORIENTED_EDGE ( 'NONE', *, *, #1947, .F. ) ;
#5963 = LINE ( 'NONE', #13243, #9288 ) ;
#5964 = CIRCLE ( 'NONE', #4735, 1.500000000000000444 ) ;
#5965 = ORIENTED_EDGE ( 'NONE', *, *, #4469, .T. ) ;
#5966 = ADVANCED_FACE ( 'NONE', ( #13435 ), #475, .F. ) ;
#5967 = VECTOR ( 'NONE', #9185, 1000.000000000000000 ) ;
#5968 = EDGE_LOOP ( 'NONE', ( #6770, #17857, #12043, #15501 ) ) ;
#5969 = VERTEX_POINT ( 'NONE', #8459 ) ;
#5970 = DIRECTION ( 'NONE',  ( -0.1566598588826321192, 0.9876526153536342445, 7.798540720466731404E-17 ) ) ;
#5971 = VECTOR ( 'NONE', #7385, 1000.000000000000000 ) ;
#5972 = CARTESIAN_POINT ( 'NONE',  ( -86.18478963674542115, 32.34879426031891114, -35.00000000000000000 ) ) ;
#5973 = ORIENTED_EDGE ( 'NONE', *, *, #4649, .F. ) ;
#5974 = VECTOR ( 'NONE', #2876, 1000.000000000000000 ) ;
#5975 = EDGE_CURVE ( 'NONE', #12855, #1506, #8037, .T. ) ;
#5976 = DIRECTION ( 'NONE',  ( -0.1566598588826321192, 0.9876526153536342445, 7.798540720466731404E-17 ) ) ;
#5977 = ORIENTED_EDGE ( 'NONE', *, *, #4671, .F. ) ;
#5978 = DIRECTION ( 'NONE',  ( -0.1566598588826321192, 0.9876526153536342445, 7.798540720466730171E-17 ) ) ;
#5979 = ORIENTED_EDGE ( 'NONE', *, *, #18052, .T. ) ;
#5980 = FACE_BOUND ( 'NONE', #10720, .T. ) ;
#5981 = AXIS2_PLACEMENT_3D ( 'NONE', #1005, #7991, #10811 ) ;
#5982 = DIRECTION ( 'NONE',  ( -0.1566598588826321192, 0.9876526153536342445, 7.798540720466730171E-17 ) ) ;
#5983 = VERTEX_POINT ( 'NONE', #12808 ) ;
#5984 = DIRECTION ( 'NONE',  ( -0.1566598588826321192, 0.9876526153536342445, 7.798540720466730171E-17 ) ) ;
#5985 = CARTESIAN_POINT ( 'NONE',  ( -64.60826822105063627, -25.43533591671226901, -21.65063509461098334 ) ) ;
#5986 = LINE ( 'NONE', #16316, #16014 ) ;
#5987 = ORIENTED_EDGE ( 'NONE', *, *, #18316, .T. ) ;
#5988 = ORIENTED_EDGE ( 'NONE', *, *, #14498, .T. ) ;
#5989 = ORIENTED_EDGE ( 'NONE', *, *, #4578, .T. ) ;
#5990 = VERTEX_POINT ( 'NONE', #9959 ) ;
#5991 = FACE_OUTER_BOUND ( 'NONE', #13739, .T. ) ;
#5992 = CARTESIAN_POINT ( 'NONE',  ( -64.77298653181324539, -88.22944028871116018, 12.99038105676661203 ) ) ;
#5993 = AXIS2_PLACEMENT_3D ( 'NONE', #1902, #9384, #6468 ) ;
#5994 = CARTESIAN_POINT ( 'NONE',  ( -76.95392591297100182, -27.39358415274517355, 1.926565525561698076E-14 ) ) ;
#5995 = ORIENTED_EDGE ( 'NONE', *, *, #7303, .F. ) ;
#5996 = EDGE_CURVE ( 'NONE', #13102, #4754, #18650, .T. ) ;
#5997 = ORIENTED_EDGE ( 'NONE', *, *, #4550, .F. ) ;
#5998 = AXIS2_PLACEMENT_3D ( 'NONE', #1692, #10312, #3106 ) ;
#5999 = ORIENTED_EDGE ( 'NONE', *, *, #4861, .T. ) ;
#6000 = EDGE_CURVE ( 'NONE', #12139, #17674, #5329, .T. ) ;
#6001 = CIRCLE ( 'NONE', #1764, 1.500000000000000444 ) ;
#6002 = AXIS2_PLACEMENT_3D ( 'NONE', #18485, #4006, #9809 ) ;
#6003 = CARTESIAN_POINT ( 'NONE',  ( -174.4298649410498854, 55.90939826654244627, 3.724467847532853426 ) ) ;
#6004 = CARTESIAN_POINT ( 'NONE',  ( -62.00000000000000000, 0.000000000000000000, -25.00000000000000000 ) ) ;
#6005 = AXIS2_PLACEMENT_3D ( 'NONE', #3371, #1778, #369 ) ;
#6006 = CARTESIAN_POINT ( 'NONE',  ( -4.361458684479201153, -15.87908452487173427, 1.561251128379126385E-14 ) ) ;
#6007 = CARTESIAN_POINT ( 'NONE',  ( -71.80233157044055758, 45.76690022515197853, -3.524781480481925744 ) ) ;
#6008 = CARTESIAN_POINT ( 'NONE',  ( -74.48479437458692587, -27.00193450553859265, -4.330127018922180326 ) ) ;
#6009 = VERTEX_POINT ( 'NONE', #9705 ) ;
#6010 = EDGE_LOOP ( 'NONE', ( #5147, #930, #10423, #2143 ) ) ;
#6011 = FACE_BOUND ( 'NONE', #12768, .T. ) ;
#6012 = DIRECTION ( 'NONE',  ( -0.1566598588826321747, 0.9876526153536343555, 0.000000000000000000 ) ) ;
#6013 = CARTESIAN_POINT ( 'NONE',  ( -75.96627329761737712, -27.23692429386254688, 21.65063509461102242 ) ) ;
#6014 = CYLINDRICAL_SURFACE ( 'NONE', #18749, 1.500000000000001554 ) ;
#6015 = ORIENTED_EDGE ( 'NONE', *, *, #10077, .T. ) ;
#6016 = CIRCLE ( 'NONE', #260, 1.500000000000000000 ) ;
#6017 = VERTEX_POINT ( 'NONE', #11370 ) ;
#6018 = VERTEX_POINT ( 'NONE', #2381 ) ;
#6019 = DIRECTION ( 'NONE',  ( 0.000000000000000000, 0.000000000000000000, 1.000000000000000000 ) ) ;
#6020 = CARTESIAN_POINT ( 'NONE',  ( -2.096680467035594297, -20.58235781331593017, 8.660254037844412167 ) ) ;
#6021 = VECTOR ( 'NONE', #6445, 1000.000000000000000 ) ;
#6022 = AXIS2_PLACEMENT_3D ( 'NONE', #10945, #3646, #13496 ) ;
#6023 = EDGE_CURVE ( 'NONE', #14160, #311, #18691, .T. ) ;
#6024 = CARTESIAN_POINT ( 'NONE',  ( -40.61513246582718040, -26.69209230973856251, 12.99038105676661736 ) ) ;
#6025 = EDGE_CURVE ( 'NONE', #202, #1113, #785, .T. ) ;
#6026 = CYLINDRICAL_SURFACE ( 'NONE', #11465, 1.500000000000001554 ) ;
#6027 = DIRECTION ( 'NONE',  ( 0.000000000000000000, 0.000000000000000000, 1.000000000000000000 ) ) ;
#6028 = EDGE_CURVE ( 'NONE', #15891, #3230, #13185, .T. ) ;
#6029 = CLOSED_SHELL ( 'NONE', ( #3434, #4803, #5007, #7101, #3019, #9319, #9262, #16192, #17067, #927 ) ) ;
#6030 = CYLINDRICAL_SURFACE ( 'NONE', #5113, 1.500000000000001554 ) ;
#6031 = DIRECTION ( 'NONE',  ( -1.000000000000000000, 0.000000000000000000, 0.000000000000000000 ) ) ;
#6032 = CYLINDRICAL_SURFACE ( 'NONE', #10731, 2.000000000000001776 ) ;
#6033 = AXIS2_PLACEMENT_3D ( 'NONE', #12933, #3082, #243 ) ;
#6034 = LINE ( 'NONE', #160, #17796 ) ;
#6035 = ORIENTED_EDGE ( 'NONE', *, *, #2994, .T. ) ;
#6036 = EDGE_LOOP ( 'NONE', ( #13311, #7927, #850, #10639 ) ) ;
#6037 = DIRECTION ( 'NONE',  ( -0.1566598588826321192, 0.9876526153536342445, 7.798540720466731404E-17 ) ) ;
#6038 = AXIS2_PLACEMENT_3D ( 'NONE', #15291, #8090, #12620 ) ;
#6039 = VECTOR ( 'NONE', #18699, 1000.000000000000000 ) ;
#6040 = VERTEX_POINT ( 'NONE', #15471 ) ;
#6041 = ORIENTED_EDGE ( 'NONE', *, *, #9746, .F. ) ;
#6042 = ORIENTED_EDGE ( 'NONE', *, *, #14752, .T. ) ;
#6043 = CIRCLE ( 'NONE', #17866, 1.500000000000000888 ) ;
#6044 = AXIS2_PLACEMENT_3D ( 'NONE', #2710, #9745, #15512 ) ;
#6045 = ORIENTED_EDGE ( 'NONE', *, *, #5490, .F. ) ;
#6046 = CIRCLE ( 'NONE', #6, 1.500000000000000444 ) ;
#6047 = DIRECTION ( 'NONE',  ( -1.000000000000000000, 0.000000000000000000, 0.000000000000000000 ) ) ;
#6048 = EDGE_CURVE ( 'NONE', #6912, #11183, #2493, .T. ) ;
#6049 = AXIS2_PLACEMENT_3D ( 'NONE', #9619, #15293, #12454 ) ;
#6050 = ADVANCED_FACE ( 'NONE', ( #8359 ), #14137, .F. ) ;
#6051 = FACE_OUTER_BOUND ( 'NONE', #7379, .T. ) ;
#6052 = DIRECTION ( 'NONE',  ( -0.9876526153536336894, -0.1566598588826349503, 0.000000000000000000 ) ) ;
#6053 = CIRCLE ( 'NONE', #7862, 144.0000000000000284 ) ;
#6054 = AXIS2_PLACEMENT_3D ( 'NONE', #9154, #14925, #1102 ) ;
#6055 = FACE_OUTER_BOUND ( 'NONE', #4037, .T. ) ;
#6056 = CARTESIAN_POINT ( 'NONE',  ( -309.1404785418517918, -2.850701963179326892, -12.83663829214475882 ) ) ;
#6057 = FACE_OUTER_BOUND ( 'NONE', #15034, .T. ) ;
#6058 = EDGE_CURVE ( 'NONE', #1680, #17205, #17142, .T. ) ;
#6059 = CARTESIAN_POINT ( 'NONE',  ( 73.09088021254186174, 1.387778780781445676E-14, 2.500000000000000444 ) ) ;
#6061 = DIRECTION ( 'NONE',  ( -0.1566598588826321192, 0.9876526153536342445, 7.798540720466731404E-17 ) ) ;
#6060 = PRODUCT_RELATED_PRODUCT_CATEGORY ( 'part', '', ( #2590 ) ) ;
#6062 = ADVANCED_FACE ( 'NONE', ( #10973 ), #12200, .F. ) ;
#6063 = VECTOR ( 'NONE', #5816, 1000.000000000000114 ) ;
#6064 = CARTESIAN_POINT ( 'NONE',  ( -60.36818477289978091, -29.82528948739120267, 4.330127018922217630 ) ) ;
#6065 = CIRCLE ( 'NONE', #16665, 1.499999999999999556 ) ;
#6067 = ORIENTED_EDGE ( 'NONE', *, *, #4948, .F. ) ;
#6066 = CYLINDRICAL_SURFACE ( 'NONE', #18164, 2.000000000000000000 ) ;
#6068 = AXIS2_PLACEMENT_3D ( 'NONE', #15866, #7432, #17218 ) ;
#6069 = VERTEX_POINT ( 'NONE', #13922 ) ;
#6070 = CARTESIAN_POINT ( 'NONE',  ( -60.36818477289977380, -29.82528948739119556, 12.99038105676661736 ) ) ;
#6071 = CIRCLE ( 'NONE', #11479, 1.500000000000000888 ) ;
#6072 = ORIENTED_EDGE ( 'NONE', *, *, #13305, .T. ) ;
#6073 = ORIENTED_EDGE ( 'NONE', *, *, #2903, .T. ) ;
#6074 = CARTESIAN_POINT ( 'NONE',  ( 0.000000000000000000, 0.000000000000000000, 30.00000000000000000 ) ) ;
#6075 = FACE_OUTER_BOUND ( 'NONE', #9010, .T. ) ;
#6076 = CIRCLE ( 'NONE', #16986, 1.500000000000000888 ) ;
#6077 = DIRECTION ( 'NONE',  ( -0.1566598588826321192, 0.9876526153536342445, 7.798540720466730171E-17 ) ) ;
#6078 = AXIS2_PLACEMENT_3D ( 'NONE', #6729, #1674, #13131 ) ;
#6079 = ORIENTED_EDGE ( 'NONE', *, *, #2240, .F. ) ;
#6080 = UNCERTAINTY_MEASURE_WITH_UNIT (LENGTH_MEASURE( 1.000000000000000082E-05 ), #10952, 'distance_accuracy_value', 'NONE');
#6081 = AXIS2_PLACEMENT_3D ( 'NONE', #6569, #12316, #11462 ) ;
#6082 = DIRECTION ( 'NONE',  ( -0.1566598588826321192, 0.9876526153536342445, 7.798540720466730171E-17 ) ) ;
#6083 = LINE ( 'NONE', #1808, #4791 ) ;
#6084 = VECTOR ( 'NONE', #7097, 1000.000000000000000 ) ;
#6085 = EDGE_LOOP ( 'NONE', ( #17561, #205, #17107, #17075 ) ) ;
#6086 = ADVANCED_FACE ( 'NONE', ( #868 ), #6646, .F. ) ;
#6087 = AXIS2_PLACEMENT_3D ( 'NONE', #7909, #4944, #17898 ) ;
#6088 = EDGE_CURVE ( 'NONE', #15023, #7569, #15610, .T. ) ;
#6089 = CARTESIAN_POINT ( 'NONE',  ( -10.28737437660097775, -16.81904367816753165, 4.330127018922214965 ) ) ;
#6090 = ORIENTED_EDGE ( 'NONE', *, *, #5044, .T. ) ;
#6091 = CARTESIAN_POINT ( 'NONE',  ( -53.94844277310118486, -28.80700040465408662, -21.65063509461098334 ) ) ;
#6092 = CARTESIAN_POINT ( 'NONE',  ( -43.08426400421124924, -27.08374195694514341, 17.32050807568881723 ) ) ;
#6093 = EDGE_CURVE ( 'NONE', #14700, #9368, #9933, .T. ) ;
#6094 = ORIENTED_EDGE ( 'NONE', *, *, #10580, .T. ) ;
#6095 = AXIS2_PLACEMENT_3D ( 'NONE', #17808, #9240, #12164 ) ;
#6096 = EDGE_LOOP ( 'NONE', ( #15238, #8034 ) ) ;
#6097 = VERTEX_POINT ( 'NONE', #18434 ) ;
#6098 = EDGE_LOOP ( 'NONE', ( #17603, #8589, #14047 ) ) ;
#6099 = CARTESIAN_POINT ( 'NONE',  ( -173.0810787726268245, 56.45151975169574143, -2.500000000000000000 ) ) ;
#6100 = FACE_BOUND ( 'NONE', #6538, .T. ) ;
#6101 = CARTESIAN_POINT ( 'NONE',  ( -26.58364252993588650, -19.40393134973095712, 4.330127018922218518 ) ) ;
#6102 = VERTEX_POINT ( 'NONE', #3673 ) ;
#6103 = DIRECTION ( 'NONE',  ( -0.9876526153536341335, 0.1566598588826326743, -0.000000000000000000 ) ) ;
#6104 = ORIENTED_EDGE ( 'NONE', *, *, #3981, .F. ) ;
#6105 = AXIS2_PLACEMENT_3D ( 'NONE', #16982, #1062, #4987 ) ;
#6106 = VERTEX_POINT ( 'NONE', #2257 ) ;
#6107 = CARTESIAN_POINT ( 'NONE',  ( -45.34904222165485521, -22.38046866850095995, 8.660254037844417496 ) ) ;
#6108 = AXIS2_PLACEMENT_3D ( 'NONE', #9100, #3296, #10509 ) ;
#6109 = DIRECTION ( 'NONE',  ( -0.1566598588826321192, 0.9876526153536342445, 7.798540720466730171E-17 ) ) ;
#6110 = DIRECTION ( 'NONE',  ( -0.9876526153536341335, -0.1566598588826327021, 0.000000000000000000 ) ) ;
#6111 = CARTESIAN_POINT ( 'NONE',  ( -90.00000000000000000, 34.99999999999999289, 35.00000000000000000 ) ) ;
#6112 = ORIENTED_EDGE ( 'NONE', *, *, #1558, .F. ) ;
#6113 = EDGE_LOOP ( 'NONE', ( #1118, #5778 ) ) ;
#6114 = CARTESIAN_POINT ( 'NONE',  ( -79.20163718375225415, 48.91533818955501545, -2.500000000000000000 ) ) ;
#6115 = ADVANCED_FACE ( 'NONE', ( #13807 ), #10967, .F. ) ;
#6116 = DIRECTION ( 'NONE',  ( -0.1566598588826321747, 0.9876526153536343555, 0.000000000000000000 ) ) ;
#6117 = CYLINDRICAL_SURFACE ( 'NONE', #854, 1.500000000000000666 ) ;
#6118 = CIRCLE ( 'NONE', #10932, 1.500000000000000888 ) ;
#6119 = ORIENTED_EDGE ( 'NONE', *, *, #6782, .F. ) ;
#6120 = CARTESIAN_POINT ( 'NONE',  ( -129.1404785418517918, -15.35070196317932911, 2.500000000000000000 ) ) ;
#6121 = ORIENTED_EDGE ( 'NONE', *, *, #12171, .T. ) ;
#6122 = ORIENTED_EDGE ( 'NONE', *, *, #8442, .T. ) ;
#6123 = FACE_OUTER_BOUND ( 'NONE', #18489, .T. ) ;
#6124 = EDGE_CURVE ( 'NONE', #16410, #3635, #2281, .T. ) ;
#6125 = EDGE_LOOP ( 'NONE', ( #750, #15116 ) ) ;
#6126 = CARTESIAN_POINT ( 'NONE',  ( -71.72618984946653597, -31.62687786454144856, 12.99038105676661736 ) ) ;
#6127 = AXIS2_PLACEMENT_3D ( 'NONE', #15225, #8222, #17056 ) ;
#6128 = AXIS2_PLACEMENT_3D ( 'NONE', #390, #4545, #10325 ) ;
#6129 = PLANE ( 'NONE',  #8516 ) ;
#6130 = FACE_OUTER_BOUND ( 'NONE', #14136, .T. ) ;
#6131 = CARTESIAN_POINT ( 'NONE',  ( -51.27495791377663181, -23.32042782179674845, 4.330127018922218518 ) ) ;
#6132 =( LENGTH_UNIT ( ) NAMED_UNIT ( * ) SI_UNIT ( .MILLI., .METRE. ) );
#6133 = EDGE_LOOP ( 'NONE', ( #11769, #14281 ) ) ;
#6134 = PRESENTATION_LAYER_ASSIGNMENT (  '', '', ( #7057 ) ) ;
#6135 = DIRECTION ( 'NONE',  ( -0.1566598588826321192, 0.9876526153536342445, 7.798540720466730171E-17 ) ) ;
#6136 = DIRECTION ( 'NONE',  ( -0.1566598588826321747, 0.9876526153536343555, 0.000000000000000000 ) ) ;
#6137 = DIRECTION ( 'NONE',  ( -0.1566598588826321192, 0.9876526153536342445, 7.798540720466731404E-17 ) ) ;
#6138 = FACE_OUTER_BOUND ( 'NONE', #14308, .T. ) ;
#6139 = ORIENTED_EDGE ( 'NONE', *, *, #9387, .F. ) ;
#6140 = ORIENTED_EDGE ( 'NONE', *, *, #18633, .F. ) ;
#6141 = CARTESIAN_POINT ( 'NONE',  ( -11.93357161039406300, -79.84813783849037350, -4.330127018922185655 ) ) ;
#6142 = ORIENTED_EDGE ( 'NONE', *, *, #2556, .F. ) ;
#6143 = ORIENTED_EDGE ( 'NONE', *, *, #5295, .F. ) ;
#6144 = ORIENTED_EDGE ( 'NONE', *, *, #18375, .F. ) ;
#6145 = EDGE_CURVE ( 'NONE', #1703, #14341, #7686, .T. ) ;
#6146 = ORIENTED_EDGE ( 'NONE', *, *, #653, .T. ) ;
#6147 = ADVANCED_FACE ( 'NONE', ( #3734 ), #15410, .F. ) ;
#6148 = EDGE_LOOP ( 'NONE', ( #7609, #18297, #6266, #4604 ) ) ;
#6149 = FACE_OUTER_BOUND ( 'NONE', #880, .T. ) ;
#6150 = DIRECTION ( 'NONE',  ( 1.000000000000000000, 0.000000000000000000, 0.000000000000000000 ) ) ;
#6151 = ORIENTED_EDGE ( 'NONE', *, *, #12161, .F. ) ;
#6152 = DIRECTION ( 'NONE',  ( -0.000000000000000000, -0.000000000000000000, -1.000000000000000000 ) ) ;
#6153 = CIRCLE ( 'NONE', #4632, 1.500000000000000888 ) ;
#6154 = CYLINDRICAL_SURFACE ( 'NONE', #16157, 1.500000000000001554 ) ;
#6155 = CARTESIAN_POINT ( 'NONE',  ( 3.231158466157545206, -19.73726462726228092, -30.00000000000000000 ) ) ;
#6156 =( NAMED_UNIT ( * ) PLANE_ANGLE_UNIT ( ) SI_UNIT ( $, .RADIAN. ) );
#6157 = CARTESIAN_POINT ( 'NONE',  ( -23.29157668696081629, -81.64972621564065491, 12.99038105676661203 ) ) ;
#6158 = EDGE_LOOP ( 'NONE', ( #1258, #6201, #7744 ) ) ;
#6159 = CARTESIAN_POINT ( 'NONE',  ( -34.19539046602859145, -25.67380322700145356, -21.65063509461098334 ) ) ;
#6160 = FACE_BOUND ( 'NONE', #11941, .T. ) ;
#6161 = DIRECTION ( 'NONE',  ( -0.1566598588826321747, 0.9876526153536343555, 0.000000000000000000 ) ) ;
#6162 = EDGE_LOOP ( 'NONE', ( #9317, #1454 ) ) ;
#6163 = DIRECTION ( 'NONE',  ( -0.9876526153536341335, -0.1566598588826327021, 0.000000000000000000 ) ) ;
#6164 = EDGE_CURVE ( 'NONE', #10299, #8719, #7159, .T. ) ;
#6166 = ORIENTED_EDGE ( 'NONE', *, *, #7425, .T. ) ;
#6165 = LINE ( 'NONE', #9183, #5117 ) ;
#6168 = ORIENTED_EDGE ( 'NONE', *, *, #15060, .T. ) ;
#6167 = ADVANCED_FACE ( 'NONE', ( #11029 ), #1040, .F. ) ;
#6169 = CARTESIAN_POINT ( 'NONE',  ( -16.91146969734005268, -22.93225569655540141, 1.887572821959364500E-14 ) ) ;
#6170 = AXIS2_PLACEMENT_3D ( 'NONE', #13806, #15338, #6639 ) ;
#6171 = CARTESIAN_POINT ( 'NONE',  ( -44.03228160938703439, -84.93958325217590755, 1.424741226644455312E-14 ) ) ;
#6172 = ORIENTED_EDGE ( 'NONE', *, *, #1975, .T. ) ;
#6173 = EDGE_LOOP ( 'NONE', ( #8847, #14361 ) ) ;
#6174 = DIRECTION ( 'NONE',  ( -0.1566598588826321192, 0.9876526153536342445, 7.798540720466730171E-17 ) ) ;
#6175 = CARTESIAN_POINT ( 'NONE',  ( -65.30644784966793281, -30.60858878180435738, 4.330127018922217630 ) ) ;
#6176 = VERTEX_POINT ( 'NONE', #13884 ) ;
#6177 = DIRECTION ( 'NONE',  ( -0.1566598588826321747, 0.9876526153536343555, 0.000000000000000000 ) ) ;
#6178 = DIRECTION ( 'NONE',  ( -0.1566598588826321192, 0.9876526153536342445, 7.798540720466730171E-17 ) ) ;
#6179 = AXIS2_PLACEMENT_3D ( 'NONE', #9349, #18103, #15135 ) ;
#6180 = CARTESIAN_POINT ( 'NONE',  ( 55.85952145814821534, 6.938893903907228378E-15, 30.00000000000000000 ) ) ;
#6181 = CARTESIAN_POINT ( 'NONE',  ( 55.85952145814821534, 6.938893903907228378E-15, 2.500000000000000000 ) ) ;
#6182 = EDGE_LOOP ( 'NONE', ( #161, #9941, #1560, #3972 ) ) ;
#6183 = DIRECTION ( 'NONE',  ( -1.000000000000000000, 0.000000000000000000, 0.000000000000000000 ) ) ;
#6184 = ORIENTED_EDGE ( 'NONE', *, *, #14460, .F. ) ;
#6185 = DIRECTION ( 'NONE',  ( -0.1566598588826321192, 0.9876526153536342445, 7.798540720466731404E-17 ) ) ;
#6186 = LINE ( 'NONE', #13368, #3585 ) ;
#6187 = ORIENTED_EDGE ( 'NONE', *, *, #2134, .T. ) ;
#6188 = VERTEX_POINT ( 'NONE', #16856 ) ;
#6189 = ORIENTED_EDGE ( 'NONE', *, *, #11337, .F. ) ;
#6190 = CYLINDRICAL_SURFACE ( 'NONE', #3499, 1.500000000000001554 ) ;
#6191 = ORIENTED_EDGE ( 'NONE', *, *, #12476, .T. ) ;
#6192 = VERTEX_POINT ( 'NONE', #14444 ) ;
#6193 = EDGE_CURVE ( 'NONE', #7789, #9740, #4202, .T. ) ;
#6194 = VERTEX_POINT ( 'NONE', #18757 ) ;
#6195 = FACE_BOUND ( 'NONE', #133, .T. ) ;
#6196 = EDGE_CURVE ( 'NONE', #18395, #7533, #4089, .T. ) ;
#6197 = ADVANCED_FACE ( 'NONE', ( #15868 ), #14447, .F. ) ;
#6198 = VERTEX_POINT ( 'NONE', #15959 ) ;
#6199 = DIRECTION ( 'NONE',  ( 0.000000000000000000, 0.000000000000000000, 1.000000000000000000 ) ) ;
#6200 = EDGE_LOOP ( 'NONE', ( #10866, #1705 ) ) ;
#6201 = ORIENTED_EDGE ( 'NONE', *, *, #7223, .T. ) ;
#6202 = ORIENTED_EDGE ( 'NONE', *, *, #9856, .T. ) ;
#6203 = ORIENTED_EDGE ( 'NONE', *, *, #14100, .T. ) ;
#6204 = DIRECTION ( 'NONE',  ( -0.1566598588826321192, 0.9876526153536342445, 7.798540720466730171E-17 ) ) ;
#6205 = DIRECTION ( 'NONE',  ( -0.9876526153536341335, -0.1566598588826327021, 0.000000000000000000 ) ) ;
#6206 = CARTESIAN_POINT ( 'NONE',  ( 0.000000000000000000, 0.000000000000000000, 30.00000000000000000 ) ) ;
#6207 = FACE_OUTER_BOUND ( 'NONE', #3217, .T. ) ;
#6208 = DIRECTION ( 'NONE',  ( -0.9876526153536341335, -0.1566598588826327021, 0.000000000000000000 ) ) ;
#6209 = VERTEX_POINT ( 'NONE', #17495 ) ;
#6210 = ORIENTED_EDGE ( 'NONE', *, *, #10296, .T. ) ;
#6211 = DIRECTION ( 'NONE',  ( -0.9857117110570272622, -0.1684411549622826243, 2.137303368083796319E-18 ) ) ;
#6212 = AXIS2_PLACEMENT_3D ( 'NONE', #17469, #4074, #7063 ) ;
#6213 = CARTESIAN_POINT ( 'NONE',  ( -309.0881213225398483, -2.850701963179330889, 18.88854657239857815 ) ) ;
#6214 = CYLINDRICAL_SURFACE ( 'NONE', #5380, 1.500000000000001554 ) ;
#6215 = ORIENTED_EDGE ( 'NONE', *, *, #3022, .T. ) ;
#6216 = ORIENTED_EDGE ( 'NONE', *, *, #8355, .F. ) ;
#6217 = DIRECTION ( 'NONE',  ( -0.9876526153536341335, -0.1566598588826327021, 0.000000000000000000 ) ) ;
#6218 = EDGE_CURVE ( 'NONE', #3442, #7107, #1994, .T. ) ;
#6219 = CARTESIAN_POINT ( 'NONE',  ( -37.15834831208948685, -26.14378280364935137, -12.99038105676658006 ) ) ;
#6220 = EDGE_CURVE ( 'NONE', #7195, #13436, #1401, .T. ) ;
#6221 = LINE ( 'NONE', #11949, #1800 ) ;
#6222 = CARTESIAN_POINT ( 'NONE',  ( -40.57549745564934085, -84.39127374608668219, -8.660254037844385522 ) ) ;
#6223 = CYLINDRICAL_SURFACE ( 'NONE', #15440, 1.500000000000001554 ) ;
#6224 = FACE_OUTER_BOUND ( 'NONE', #688, .T. ) ;
#6225 = ADVANCED_FACE ( 'NONE', ( #7219 ), #16851, .F. ) ;
#6226 = LINE ( 'NONE', #437, #15588 ) ;
#6227 = ORIENTED_EDGE ( 'NONE', *, *, #704, .T. ) ;
#6228 = ORIENTED_EDGE ( 'NONE', *, *, #11365, .F. ) ;
#6229 = CARTESIAN_POINT ( 'NONE',  ( -15.39035576413176187, -80.39644734457957043, -12.99038105676658539 ) ) ;
#6230 = EDGE_LOOP ( 'NONE', ( #17355, #6757, #16475, #17090 ) ) ;
#6231 = EDGE_LOOP ( 'NONE', ( #12143, #18498 ) ) ;
#6232 = DIRECTION ( 'NONE',  ( 0.9876526153536341335, -0.1566598588826326743, 3.168663947239273463E-17 ) ) ;
#6233 = CARTESIAN_POINT ( 'NONE',  ( -9.299721761247353058, -16.66238381928489787, -17.32050807568878170 ) ) ;
#6234 = AXIS2_PLACEMENT_3D ( 'NONE', #2963, #11488, #10265 ) ;
#6235 = ORIENTED_EDGE ( 'NONE', *, *, #598, .F. ) ;
#6236 = CARTESIAN_POINT ( 'NONE',  ( -69.99999999999998579, -45.00000000000000711, -19.99999999999999645 ) ) ;
#6237 = LINE ( 'NONE', #14850, #15170 ) ;
#6238 = AXIS2_PLACEMENT_3D ( 'NONE', #7167, #5741, #10163 ) ;
#6239 = EDGE_CURVE ( 'NONE', #3635, #16410, #16217, .T. ) ;
#6240 = CARTESIAN_POINT ( 'NONE',  ( 7.819480696678551723, -76.71494066083772623, -4.330127018922189208 ) ) ;
#6241 = CARTESIAN_POINT ( 'NONE',  ( -57.20087360589841552, -24.26038697509254050, 1.926565525561698076E-14 ) ) ;
#6242 = CARTESIAN_POINT ( 'NONE',  ( -40.61513246582718750, -26.69209230973856251, -12.99038105676658006 ) ) ;
#6243 = ORIENTED_EDGE ( 'NONE', *, *, #6533, .F. ) ;
#6244 = DIRECTION ( 'NONE',  ( -0.1566598588826321192, 0.9876526153536342445, 7.798540720466730171E-17 ) ) ;
#6245 = AXIS2_PLACEMENT_3D ( 'NONE', #12082, #10755, #13420 ) ;
#6246 = VERTEX_POINT ( 'NONE', #10038 ) ;
#6247 = DIRECTION ( 'NONE',  ( -0.1566598588826321747, 0.9876526153536343555, 0.000000000000000000 ) ) ;
#6248 = FACE_BOUND ( 'NONE', #1755, .T. ) ;
#6249 = EDGE_CURVE ( 'NONE', #11583, #6259, #17733, .T. ) ;
#6250 = DIRECTION ( 'NONE',  ( 0.000000000000000000, 0.000000000000000000, 1.000000000000000000 ) ) ;
#6251 = FACE_OUTER_BOUND ( 'NONE', #16611, .T. ) ;
#6253 = EDGE_LOOP ( 'NONE', ( #2810, #2206 ) ) ;
#6252 = CARTESIAN_POINT ( 'NONE',  ( -53.90880776292333820, -86.50618184100220276, -17.32050807568878525 ) ) ;
#6254 = EDGE_LOOP ( 'NONE', ( #11787, #16718 ) ) ;
#6255 = CARTESIAN_POINT ( 'NONE',  ( -126.1404785418517918, 9.595891400605990995, 2.500000000000000000 ) ) ;
#6256 = AXIS2_PLACEMENT_3D ( 'NONE', #5325, #14125, #1472 ) ;
#6257 = ORIENTED_EDGE ( 'NONE', *, *, #11692, .T. ) ;
#6258 = ORIENTED_EDGE ( 'NONE', *, *, #4649, .T. ) ;
#6259 = VERTEX_POINT ( 'NONE', #13829 ) ;
#6260 = CARTESIAN_POINT ( 'NONE',  ( -172.7326993491721225, 43.83249341393818810, 9.951701414186830458E-16 ) ) ;
#6261 = ORIENTED_EDGE ( 'NONE', *, *, #2780, .F. ) ;
#6262 = VECTOR ( 'NONE', #6816, 1000.000000000000000 ) ;
#6263 = DIRECTION ( 'NONE',  ( -0.1566598588826321192, 0.9876526153536342445, 7.798540720466730171E-17 ) ) ;
#6264 = ADVANCED_FACE ( 'NONE', ( #14118 ), #14327, .F. ) ;
#6265 = DIRECTION ( 'NONE',  ( -0.9876526153536341335, -0.1566598588826327021, 0.000000000000000000 ) ) ;
#6266 = ORIENTED_EDGE ( 'NONE', *, *, #8837, .T. ) ;
#6267 = DIRECTION ( 'NONE',  ( -0.1566598588826321192, 0.9876526153536342445, 7.798540720466731404E-17 ) ) ;
#6268 = DIRECTION ( 'NONE',  ( -0.9876526153536336894, -0.1566598588826349503, 0.000000000000000000 ) ) ;
#6269 = EDGE_CURVE ( 'NONE', #5835, #1839, #10130, .T. ) ;
#6270 = CARTESIAN_POINT ( 'NONE',  ( -128.4427290061107101, -15.07742888475873677, -3.566331213966875691 ) ) ;
#6271 = EDGE_CURVE ( 'NONE', #15200, #753, #10427, .T. ) ;
#6272 = CARTESIAN_POINT ( 'NONE',  ( 3.231158466157545206, -19.73726462726228092, -30.00000000000000000 ) ) ;
#6273 = CARTESIAN_POINT ( 'NONE',  ( -77.18258565727084886, 4.450738551673815380, -20.00000000000000355 ) ) ;
#6274 = DIRECTION ( 'NONE',  ( -0.1566598588826321192, 0.9876526153536342445, 7.798540720466730171E-17 ) ) ;
#6275 = ORIENTED_EDGE ( 'NONE', *, *, #16312, .T. ) ;
#6276 = EDGE_CURVE ( 'NONE', #7482, #14323, #7787, .T. ) ;
#6277 = CARTESIAN_POINT ( 'NONE',  ( -75.96627329761737712, -27.23692429386252911, -21.65063509461097979 ) ) ;
#6278 = ORIENTED_EDGE ( 'NONE', *, *, #662, .T. ) ;
#6279 = DIRECTION ( 'NONE',  ( -0.1566598588826321192, 0.9876526153536342445, 7.798540720466730171E-17 ) ) ;
#6280 = AXIS2_PLACEMENT_3D ( 'NONE', #2414, #13973, #15294 ) ;
#6281 = PRODUCT_RELATED_PRODUCT_CATEGORY ( 'part', '', ( #12080 ) ) ;
#6282 = AXIS2_PLACEMENT_3D ( 'NONE', #13022, #10169, #5845 ) ;
#6283 = DIRECTION ( 'NONE',  ( -1.000000000000000000, 0.000000000000000000, 0.000000000000000000 ) ) ;
#6284 = EDGE_LOOP ( 'NONE', ( #4377, #6258 ) ) ;
#6285 = AXIS2_PLACEMENT_3D ( 'NONE', #14666, #16380, #13413 ) ;
#6286 = EDGE_LOOP ( 'NONE', ( #17721, #6971 ) ) ;
#6287 = EDGE_LOOP ( 'NONE', ( #7436, #5026, #18206, #10647 ) ) ;
#6288 = EDGE_LOOP ( 'NONE', ( #15699, #15812, #6461, #4492 ) ) ;
#6289 = DIRECTION ( 'NONE',  ( -0.1566598588826321192, 0.9876526153536342445, 7.798540720466730171E-17 ) ) ;
#6290 = AXIS2_PLACEMENT_3D ( 'NONE', #8781, #11686, #4507 ) ;
#6291 = ORIENTED_EDGE ( 'NONE', *, *, #4849, .T. ) ;
#6292 = FACE_BOUND ( 'NONE', #18522, .T. ) ;
#6293 = DIRECTION ( 'NONE',  ( -0.1566598588826321192, 0.9876526153536342445, 7.798540720466731404E-17 ) ) ;
#6294 = AXIS2_PLACEMENT_3D ( 'NONE', #8752, #1569, #7357 ) ;
#6295 = AXIS2_PLACEMENT_3D ( 'NONE', #8200, #15292, #18379 ) ;
#6296 = EDGE_CURVE ( 'NONE', #13205, #4027, #17669, .T. ) ;
#6297 = EDGE_LOOP ( 'NONE', ( #18793, #15354 ) ) ;
#6298 = FACE_BOUND ( 'NONE', #10316, .T. ) ;
#6299 = CIRCLE ( 'NONE', #540, 1.500000000000000888 ) ;
#6300 = CYLINDRICAL_SURFACE ( 'NONE', #1824, 1.500000000000001554 ) ;
#6301 = CARTESIAN_POINT ( 'NONE',  ( -2.000000000000000000, 0.000000000000000000, 30.00000000000000000 ) ) ;
#6302 = EDGE_CURVE ( 'NONE', #13704, #5893, #11655, .T. ) ;
#6303 = LINE ( 'NONE', #15191, #2688 ) ;
#6304 = DIRECTION ( 'NONE',  ( -0.9876526153536336894, -0.1566598588826349503, 0.000000000000000000 ) ) ;
#6305 = CYLINDRICAL_SURFACE ( 'NONE', #8379, 1.500000000000001554 ) ;
#6306 = ORIENTED_EDGE ( 'NONE', *, *, #7990, .F. ) ;
#6307 = ORIENTED_EDGE ( 'NONE', *, *, #4516, .F. ) ;
#6308 = CARTESIAN_POINT ( 'NONE',  ( -175.0988807681447383, 56.35851375132025254, 2.556294622946508611E-15 ) ) ;
#6309 = DIRECTION ( 'NONE',  ( 0.000000000000000000, 0.000000000000000000, 1.000000000000000000 ) ) ;
#6310 = ORIENTED_EDGE ( 'NONE', *, *, #3098, .T. ) ;
#6311 = CARTESIAN_POINT ( 'NONE',  ( -85.13801595139509004, -33.83333333333328596, -30.00000000000000000 ) ) ;
#6312 = AXIS2_PLACEMENT_3D ( 'NONE', #8046, #11063, #864 ) ;
#6313 = DIRECTION ( 'NONE',  ( -0.1566598588826321192, 0.9876526153536342445, 7.798540720466730171E-17 ) ) ;
#6314 = ORIENTED_EDGE ( 'NONE', *, *, #17862, .T. ) ;
#6315 = DIRECTION ( 'NONE',  ( -0.9876526153536341335, -0.1566598588826327021, 0.000000000000000000 ) ) ;
#6316 = ORIENTED_EDGE ( 'NONE', *, *, #8069, .F. ) ;
#6317 = VECTOR ( 'NONE', #16282, 1000.000000000000000 ) ;
#6318 = DIRECTION ( 'NONE',  ( -0.9876526153536341335, -0.1566598588826327021, 0.000000000000000000 ) ) ;
#6319 = AXIS2_PLACEMENT_3D ( 'NONE', #14878, #3206, #4094 ) ;
#6320 = CYLINDRICAL_SURFACE ( 'NONE', #9061, 20.00000000000001066 ) ;
#6321 = DIRECTION ( 'NONE',  ( -0.9876526153536341335, -0.1566598588826327021, 0.000000000000000000 ) ) ;
#6322 = COLOUR_RGB ( '', 0.31764706, 0.68627451, 0.89019608) ;
#6323 = ORIENTED_EDGE ( 'NONE', *, *, #15525, .F. ) ;
#6324 = DIRECTION ( 'NONE',  ( -0.1566598588826321192, 0.9876526153536342445, 7.798540720466731404E-17 ) ) ;
#6325 = CARTESIAN_POINT ( 'NONE',  ( -25.80034323552273179, -24.34219442649909126, 4.330127018922217630 ) ) ;
#6326 = EDGE_CURVE ( 'NONE', #7929, #11102, #183, .T. ) ;
#6327 = CARTESIAN_POINT ( 'NONE',  ( -26.74836084069850983, -82.19803572172985184, -12.99038105676658539 ) ) ;
#6328 = ORIENTED_EDGE ( 'NONE', *, *, #5128, .T. ) ;
#6329 = CYLINDRICAL_SURFACE ( 'NONE', #6095, 1.500000000000001554 ) ;
#6330 = ADVANCED_FACE ( 'NONE', ( #13652 ), #695, .F. ) ;
#6331 = CIRCLE ( 'NONE', #16931, 1.500000000000000888 ) ;
#6332 = ORIENTED_EDGE ( 'NONE', *, *, #13511, .T. ) ;
#6333 = VECTOR ( 'NONE', #3103, 1000.000000000000000 ) ;
#6334 = CARTESIAN_POINT ( 'NONE',  ( -34.68921677370540380, -25.75213315644277046, 1.869203119972154228E-14 ) ) ;
#6335 = EDGE_CURVE ( 'NONE', #7658, #2224, #2007, .T. ) ;
#6336 = AXIS2_PLACEMENT_3D ( 'NONE', #10804, #508, #16441 ) ;
#6337 = EDGE_LOOP ( 'NONE', ( #445, #1075, #6599, #7226 ) ) ;
#6338 = DIRECTION ( 'NONE',  ( 3.816390434826605238E-17, 0.000000000000000000, -1.000000000000000000 ) ) ;
#6339 = CARTESIAN_POINT ( 'NONE',  ( -11.76885329963143434, -17.05403346649147522, -21.65063509461097979 ) ) ;
#6340 = VECTOR ( 'NONE', #3394, 1000.000000000000000 ) ;
#6341 = DIRECTION ( 'NONE',  ( -0.9876526153536336894, -0.1566598588826349503, 0.000000000000000000 ) ) ;
#6342 = CARTESIAN_POINT ( 'NONE',  ( -75.96627329761737712, -27.23692429386252911, -21.65063509461097979 ) ) ;
#6343 = CYLINDRICAL_SURFACE ( 'NONE', #1920, 1.500000000000000666 ) ;
#6344 = VECTOR ( 'NONE', #5336, 1000.000000000000000 ) ;
#6345 = ORIENTED_EDGE ( 'NONE', *, *, #2716, .T. ) ;
#6346 = CARTESIAN_POINT ( 'NONE',  ( -21.84973277410820458, -23.71555499096855613, -17.32050807568878170 ) ) ;
#6347 = AXIS2_PLACEMENT_3D ( 'NONE', #9752, #9910, #11043 ) ;
#6348 = DIRECTION ( 'NONE',  ( 0.000000000000000000, 0.000000000000000000, 1.000000000000000000 ) ) ;
#6349 = AXIS2_PLACEMENT_3D ( 'NONE', #1971, #9263, #11809 ) ;
#6350 = DIRECTION ( 'NONE',  ( -0.1566598588826321192, 0.9876526153536342445, 7.798540720466730171E-17 ) ) ;
#6351 = CARTESIAN_POINT ( 'NONE',  ( -53.90880776292332399, -86.50618184100223118, 17.32050807568881368 ) ) ;
#6352 = EDGE_LOOP ( 'NONE', ( #16119, #1329 ) ) ;
#6353 = DIRECTION ( 'NONE',  ( -0.9876526153536341335, -0.1566598588826327021, 0.000000000000000000 ) ) ;
#6354 = FACE_OUTER_BOUND ( 'NONE', #10669, .T. ) ;
#6356 = ORIENTED_EDGE ( 'NONE', *, *, #5686, .F. ) ;
#6355 = FACE_OUTER_BOUND ( 'NONE', #2680, .T. ) ;
#6357 = CIRCLE ( 'NONE', #4807, 1.500000000000000888 ) ;
#6358 = FACE_OUTER_BOUND ( 'NONE', #5010, .T. ) ;
#6359 = EDGE_CURVE ( 'NONE', #10712, #15083, #10051, .T. ) ;
#6360 = CIRCLE ( 'NONE', #4809, 1.500000000000000888 ) ;
#6361 = ORIENTED_EDGE ( 'NONE', *, *, #1877, .T. ) ;
#6362 = VERTEX_POINT ( 'NONE', #6334 ) ;
#6363 = CIRCLE ( 'NONE', #14518, 1.499999999999999556 ) ;
#6364 = AXIS2_PLACEMENT_3D ( 'NONE', #1345, #14217, #2915 ) ;
#6365 = DIRECTION ( 'NONE',  ( -0.000000000000000000, -0.000000000000000000, -1.000000000000000000 ) ) ;
#6366 = EDGE_CURVE ( 'NONE', #10934, #6176, #8673, .T. ) ;
#6367 = CARTESIAN_POINT ( 'NONE',  ( -15.39035576413176187, -80.39644734457958464, 21.65063509461101532 ) ) ;
#6368 = CARTESIAN_POINT ( 'NONE',  ( -23.33121169713865584, -23.95054477929251036, 17.32050807568881723 ) ) ;
#6369 = CARTESIAN_POINT ( 'NONE',  ( -21.64537945316773460, -18.62063205531779886, 4.330127018922218518 ) ) ;
#6370 = AXIS2_PLACEMENT_3D ( 'NONE', #2348, #2457, #12261 ) ;
#6371 = DIRECTION ( 'NONE',  ( -0.9876526153536341335, -0.1566598588826327021, 0.000000000000000000 ) ) ;
#6372 = AXIS2_PLACEMENT_3D ( 'NONE', #3331, #9135, #6110 ) ;
#6373 = LINE ( 'NONE', #13255, #6340 ) ;
#6374 = FACE_OUTER_BOUND ( 'NONE', #15680, .T. ) ;
#6375 = EDGE_LOOP ( 'NONE', ( #10523, #17326 ) ) ;
#6376 = FACE_BOUND ( 'NONE', #18173, .T. ) ;
#6377 = AXIS2_PLACEMENT_3D ( 'NONE', #12131, #9217, #7800 ) ;
#6378 = CARTESIAN_POINT ( 'NONE',  ( 0.000000000000000000, 0.000000000000000000, 30.00000000000000000 ) ) ;
#6379 = ORIENTED_EDGE ( 'NONE', *, *, #11615, .F. ) ;
#6380 = DIRECTION ( 'NONE',  ( -0.9876526153536341335, -0.1566598588826327021, 0.000000000000000000 ) ) ;
#6381 = VECTOR ( 'NONE', #4767, 1000.000000000000000 ) ;
#6382 = DIRECTION ( 'NONE',  ( -0.1566598588826321192, 0.9876526153536342445, 7.798540720466730171E-17 ) ) ;
#6383 = ORIENTED_EDGE ( 'NONE', *, *, #11287, .F. ) ;
#6384 = EDGE_LOOP ( 'NONE', ( #853, #5228, #6227, #15566 ) ) ;
#6385 = VERTEX_POINT ( 'NONE', #16741 ) ;
#6386 = CARTESIAN_POINT ( 'NONE',  ( -15.92381708198642798, -22.77559583767277473, -12.99038105676658006 ) ) ;
#6387 = ADVANCED_FACE ( 'NONE', ( #5253 ), #623, .F. ) ;
#6388 = EDGE_CURVE ( 'NONE', #9162, #10150, #2901, .T. ) ;
#6389 = AXIS2_PLACEMENT_3D ( 'NONE', #7948, #3045, #11641 ) ;
#6390 = FACE_BOUND ( 'NONE', #12095, .T. ) ;
#6391 = EDGE_CURVE ( 'NONE', #8304, #16372, #7758, .T. ) ;
#6392 = CIRCLE ( 'NONE', #11777, 15.78184964806336055 ) ;
#6393 = FILL_AREA_STYLE_COLOUR ( '', #13089 ) ;
#6394 = AXIS2_PLACEMENT_3D ( 'NONE', #3479, #7767, #12104 ) ;
#6395 = EDGE_LOOP ( 'NONE', ( #12612, #1090, #11232, #6314 ) ) ;
#6396 = ORIENTED_EDGE ( 'NONE', *, *, #15746, .F. ) ;
#6397 = DIRECTION ( 'NONE',  ( -0.9876526153536336894, -0.1566598588826349503, 0.000000000000000000 ) ) ;
#6398 = EDGE_LOOP ( 'NONE', ( #10502, #15851 ) ) ;
#6399 = DIRECTION ( 'NONE',  ( -0.9876526153536336894, -0.1566598588826349503, 0.000000000000000000 ) ) ;
#6401 = DIRECTION ( 'NONE',  ( -0.9876526153536341335, -0.1566598588826327021, 0.000000000000000000 ) ) ;
#6400 = VECTOR ( 'NONE', #11514, 1000.000000000000000 ) ;
#6402 = FACE_OUTER_BOUND ( 'NONE', #13109, .T. ) ;
#6403 = CARTESIAN_POINT ( 'NONE',  ( -73.42100199588526266, 46.45565180342956779, -2.660647884740717561 ) ) ;
#6404 = ORIENTED_EDGE ( 'NONE', *, *, #1852, .F. ) ;
#6405 = VERTEX_POINT ( 'NONE', #16428 ) ;
#6406 = DIRECTION ( 'NONE',  ( 1.000000000000000000, 0.000000000000000000, 0.000000000000000000 ) ) ;
#6407 = ADVANCED_FACE ( 'NONE', ( #5991 ), #12122, .F. ) ;
#6408 = CARTESIAN_POINT ( 'NONE',  ( -78.43540483600145308, -27.62857394106911002, -17.32050807568878170 ) ) ;
#6409 = B_SPLINE_CURVE_WITH_KNOTS ( 'NONE', 3,
 ( #4434, #96, #1161, #4152 ),
 .UNSPECIFIED., .F., .F.,
 ( 4, 4 ),
 ( 0.000000000000000000, 0.003000475340473870295 ),
 .UNSPECIFIED. ) ;
#6410 = ADVANCED_FACE ( 'NONE', ( #4654 ), #14893, .F. ) ;
#6411 = VERTEX_POINT ( 'NONE', #1916 ) ;
#6412 = ORIENTED_EDGE ( 'NONE', *, *, #14761, .F. ) ;
#6413 = DIRECTION ( 'NONE',  ( 1.000000000000000000, 0.000000000000000000, 0.000000000000000000 ) ) ;
#6414 = VERTEX_POINT ( 'NONE', #595 ) ;
#6415 = DIRECTION ( 'NONE',  ( -0.1566598588826321747, 0.9876526153536343555, 0.000000000000000000 ) ) ;
#6416 = AXIS2_PLACEMENT_3D ( 'NONE', #18472, #17398, #2859 ) ;
#6417 = DIRECTION ( 'NONE',  ( -0.9876526153536336894, -0.1566598588826349503, 0.000000000000000000 ) ) ;
#6418 = PLANE ( 'NONE',  #5755 ) ;
#6419 =( NAMED_UNIT ( * ) PLANE_ANGLE_UNIT ( ) SI_UNIT ( $, .RADIAN. ) );
#6420 = ORIENTED_EDGE ( 'NONE', *, *, #16102, .F. ) ;
#6421 = DIRECTION ( 'NONE',  ( 0.000000000000000000, 0.000000000000000000, 1.000000000000000000 ) ) ;
#6422 = DIRECTION ( 'NONE',  ( -0.1566598588826321192, 0.9876526153536342445, 7.798540720466730171E-17 ) ) ;
#6423 = VECTOR ( 'NONE', #1511, 1000.000000000000000 ) ;
#6424 = AXIS2_PLACEMENT_3D ( 'NONE', #17319, #2955, #15861 ) ;
#6425 = CYLINDRICAL_SURFACE ( 'NONE', #11031, 1.500000000000001554 ) ;
#6426 = ORIENTED_EDGE ( 'NONE', *, *, #10838, .T. ) ;
#6427 = VERTEX_POINT ( 'NONE', #3135 ) ;
#6428 = CARTESIAN_POINT ( 'NONE',  ( 7.819480696678551723, -76.71494066083772623, 12.99038105676660493 ) ) ;
#6429 = ORIENTED_EDGE ( 'NONE', *, *, #8088, .T. ) ;
#6430 = EDGE_LOOP ( 'NONE', ( #12252, #18428 ) ) ;
#6431 = ORIENTED_EDGE ( 'NONE', *, *, #11947, .F. ) ;
#6432 = VECTOR ( 'NONE', #13714, 1000.000000000000000 ) ;
#6433 = EDGE_LOOP ( 'NONE', ( #424, #5699 ) ) ;
#6434 = CARTESIAN_POINT ( 'NONE',  ( -62.00000000000000000, 0.000000000000000000, -20.00000000000000000 ) ) ;
#6435 = CARTESIAN_POINT ( 'NONE',  ( -1.109027851681966492, -20.42569795443330349, -12.99038105676658361 ) ) ;
#6436 = EDGE_CURVE ( 'NONE', #855, #16087, #5947, .T. ) ;
#6437 = ORIENTED_EDGE ( 'NONE', *, *, #13859, .T. ) ;
#6438 = VECTOR ( 'NONE', #18254, 1000.000000000000000 ) ;
#6439 = CARTESIAN_POINT ( 'NONE',  ( -53.90880776292333820, -86.50618184100221697, 8.660254037844412167 ) ) ;
#6440 = EDGE_CURVE ( 'NONE', #3894, #11326, #11069, .T. ) ;
#6441 = DIRECTION ( 'NONE',  ( -0.000000000000000000, -0.000000000000000000, -1.000000000000000000 ) ) ;
#6442 = DIRECTION ( 'NONE',  ( 1.000000000000000000, -0.000000000000000000, -0.000000000000000000 ) ) ;
#6443 = DIRECTION ( 'NONE',  ( -0.9876526153536344665, -0.1566598588826304539, 0.000000000000000000 ) ) ;
#6444 = ADVANCED_FACE ( 'NONE', ( #13178 ), #6190, .F. ) ;
#6445 = DIRECTION ( 'NONE',  ( -0.1566598588826321192, 0.9876526153536342445, 7.798540720466730171E-17 ) ) ;
#6446 = DIRECTION ( 'NONE',  ( -0.1566598588826321192, 0.9876526153536342445, 7.798540720466730171E-17 ) ) ;
#6447 = DIRECTION ( 'NONE',  ( -0.9876526153536336894, -0.1566598588826350336, 0.000000000000000000 ) ) ;
#6448 = EDGE_LOOP ( 'NONE', ( #13683, #7326, #3689, #5031, #13136, #11872, #406 ) ) ;
#6449 = CARTESIAN_POINT ( 'NONE',  ( -5.059638313096497697, -21.05233738996382797, -17.32050807568878170 ) ) ;
#6450 = DIRECTION ( 'NONE',  ( -0.1566598588826321747, 0.9876526153536343555, 0.000000000000000000 ) ) ;
#6451 = ORIENTED_EDGE ( 'NONE', *, *, #5760, .T. ) ;
#6452 = DIRECTION ( 'NONE',  ( 0.000000000000000000, 0.000000000000000000, 1.000000000000000000 ) ) ;
#6453 = FACE_OUTER_BOUND ( 'NONE', #6230, .T. ) ;
#6454 = ORIENTED_EDGE ( 'NONE', *, *, #18785, .T. ) ;
#6455 = DIRECTION ( 'NONE',  ( 0.000000000000000000, 0.000000000000000000, 1.000000000000000000 ) ) ;
#6456 = AXIS2_PLACEMENT_3D ( 'NONE', #2280, #3978, #6852 ) ;
#6457 = VERTEX_POINT ( 'NONE', #2001 ) ;
#6458 = LINE ( 'NONE', #2350, #10025 ) ;
#6459 = EDGE_LOOP ( 'NONE', ( #2094, #13710 ) ) ;
#6460 = DIRECTION ( 'NONE',  ( -0.1566598588826321192, 0.9876526153536342445, 7.798540720466730171E-17 ) ) ;
#6461 = ORIENTED_EDGE ( 'NONE', *, *, #359, .F. ) ;
#6462 = CYLINDRICAL_SURFACE ( 'NONE', #18218, 1.500000000000001554 ) ;
#6463 = PLANE ( 'NONE',  #13657 ) ;
#6464 = UNCERTAINTY_MEASURE_WITH_UNIT (LENGTH_MEASURE( 1.000000000000000082E-05 ), #8318, 'distance_accuracy_value', 'NONE');
#6465 = EDGE_CURVE ( 'NONE', #10326, #6414, #7172, .T. ) ;
#6466 = DIRECTION ( 'NONE',  ( -0.9826218788918642533, -0.1856185419698762884, 0.000000000000000000 ) ) ;
#6467 = ORIENTED_EDGE ( 'NONE', *, *, #833, .F. ) ;
#6468 = DIRECTION ( 'NONE',  ( 0.000000000000000000, 0.000000000000000000, 1.000000000000000000 ) ) ;
#6469 = ORIENTED_EDGE ( 'NONE', *, *, #13408, .T. ) ;
#6470 = CARTESIAN_POINT ( 'NONE',  ( -60.16383145195930382, -24.73036655174043830, 17.32050807568881723 ) ) ;
#6471 = ADVANCED_FACE ( 'NONE', ( #14704 ), #1721, .F. ) ;
#6472 = DIRECTION ( 'NONE',  ( 0.000000000000000000, 0.000000000000000000, 1.000000000000000000 ) ) ;
#6473 = EDGE_CURVE ( 'NONE', #17580, #15127, #190, .T. ) ;
#6474 = ORIENTED_EDGE ( 'NONE', *, *, #9956, .F. ) ;
#6475 = ORIENTED_EDGE ( 'NONE', *, *, #3561, .T. ) ;
#6476 = VERTEX_POINT ( 'NONE', #16224 ) ;
#6477 = FACE_OUTER_BOUND ( 'NONE', #18643, .T. ) ;
#6478 = ORIENTED_EDGE ( 'NONE', *, *, #16016, .T. ) ;
#6479 = FACE_BOUND ( 'NONE', #4848, .T. ) ;
#6480 = CARTESIAN_POINT ( 'NONE',  ( -13.25033222266188915, -17.28902325481542235, -12.99038105676658006 ) ) ;
#6481 = ORIENTED_EDGE ( 'NONE', *, *, #11786, .T. ) ;
#6482 = EDGE_CURVE ( 'NONE', #862, #8986, #3192, .T. ) ;
#6483 = CARTESIAN_POINT ( 'NONE',  ( -19.17624791478365864, -18.22898240811121795, 17.32050807568881368 ) ) ;
#6484 = FACE_BOUND ( 'NONE', #6286, .T. ) ;
#6485 = CARTESIAN_POINT ( 'NONE',  ( -39.09401853261888959, -84.15628395776272441, -8.660254037844385522 ) ) ;
#6486 = CARTESIAN_POINT ( 'NONE',  ( -41.39843176024034221, -21.75382923297042481, -21.65063509461097979 ) ) ;
#6488 = EDGE_CURVE ( 'NONE', #13205, #2144, #8365, .T. ) ;
#6487 = DIRECTION ( 'NONE',  ( -0.1566598588826321192, 0.9876526153536342445, 7.798540720466731404E-17 ) ) ;
#6489 = DIRECTION ( 'NONE',  ( -0.1566598588826321192, 0.9876526153536342445, 7.798540720466730171E-17 ) ) ;
#6490 = EDGE_LOOP ( 'NONE', ( #9178, #10360 ) ) ;
#6491 = ORIENTED_EDGE ( 'NONE', *, *, #1349, .T. ) ;
#6492 = DIRECTION ( 'NONE',  ( -0.1566598588826321192, 0.9876526153536342445, 7.798540720466730171E-17 ) ) ;
#6493 = ADVANCED_FACE ( 'NONE', ( #10339 ), #14711, .T. ) ;
#6494 = CARTESIAN_POINT ( 'NONE',  ( -76.66445292623467367, -32.41017715895461038, 4.330127018922217630 ) ) ;
#6495 = ORIENTED_EDGE ( 'NONE', *, *, #2052, .F. ) ;
#6496 = DIRECTION ( 'NONE',  ( -0.1566598588826321192, 0.9876526153536342445, 7.798540720466730171E-17 ) ) ;
#6497 = DIRECTION ( 'NONE',  ( 1.000000000000000000, -3.469446951953611033E-15, 0.000000000000000000 ) ) ;
#6498 = CARTESIAN_POINT ( 'NONE',  ( -174.3141932433752004, 55.97754034394239397, -3.563338245596195719 ) ) ;
#6499 = ORIENTED_EDGE ( 'NONE', *, *, #16137, .T. ) ;
#6500 = CARTESIAN_POINT ( 'NONE',  ( -25.10216360690543524, -19.16894156140701355, 4.330127018922218518 ) ) ;
#6501 = DIRECTION ( 'NONE',  ( -0.000000000000000000, -0.000000000000000000, -1.000000000000000000 ) ) ;
#6502 = CARTESIAN_POINT ( 'NONE',  ( -6.830590222863280658, -16.27073417207831696, 12.99038105676661026 ) ) ;
#6503 = ADVANCED_FACE ( 'NONE', ( #7508 ), #13375, .F. ) ;
#6504 = ADVANCED_FACE ( 'NONE', ( #10525 ), #17860, .F. ) ;
#6505 = EDGE_CURVE ( 'NONE', #14684, #8813, #15356, .T. ) ;
#6506 = DIRECTION ( 'NONE',  ( -0.1566598588826321192, 0.9876526153536342445, 7.798540720466731404E-17 ) ) ;
#6507 = AXIS2_PLACEMENT_3D ( 'NONE', #4030, #12851, #773 ) ;
#6508 = DIRECTION ( 'NONE',  ( -0.9876526153536341335, -0.1566598588826327021, 0.000000000000000000 ) ) ;
#6509 = PLANE ( 'NONE',  #5756 ) ;
#6510 = DIRECTION ( 'NONE',  ( 0.000000000000000000, 0.000000000000000000, 1.000000000000000000 ) ) ;
#6511 = ORIENTED_EDGE ( 'NONE', *, *, #1694, .F. ) ;
#6512 = EDGE_LOOP ( 'NONE', ( #16847, #16183, #10652, #226 ) ) ;
#6513 = DIRECTION ( 'NONE',  ( 0.000000000000000000, -1.000000000000000000, 0.000000000000000000 ) ) ;
#6514 = ORIENTED_EDGE ( 'NONE', *, *, #4514, .F. ) ;
#6515 = ORIENTED_EDGE ( 'NONE', *, *, #7985, .F. ) ;
#6516 = DIRECTION ( 'NONE',  ( -0.1566598588826321192, 0.9876526153536342445, 7.798540720466730171E-17 ) ) ;
#6517 = EDGE_LOOP ( 'NONE', ( #10049, #7722, #15650, #14614 ) ) ;
#6518 = ORIENTED_EDGE ( 'NONE', *, *, #4723, .T. ) ;
#6519 = VERTEX_POINT ( 'NONE', #16903 ) ;
#6520 = AXIS2_PLACEMENT_3D ( 'NONE', #16264, #18085, #10737 ) ;
#6521 = FACE_OUTER_BOUND ( 'NONE', #1977, .T. ) ;
#6522 = CARTESIAN_POINT ( 'NONE',  ( -84.16561914167411373, 33.60000000000000142, 30.00000000000000000 ) ) ;
#6523 = DIRECTION ( 'NONE',  ( 1.000000000000000000, 0.000000000000000000, 0.000000000000000000 ) ) ;
#6524 = ORIENTED_EDGE ( 'NONE', *, *, #3416, .F. ) ;
#6525 = DIRECTION ( 'NONE',  ( -0.9876526153536341335, -0.1566598588826327021, 0.000000000000000000 ) ) ;
#6526 = DIRECTION ( 'NONE',  ( -0.000000000000000000, -0.000000000000000000, -1.000000000000000000 ) ) ;
#6527 = CARTESIAN_POINT ( 'NONE',  ( -43.86756329862440396, -22.14547888017701638, 17.32050807568882078 ) ) ;
#6528 = CYLINDRICAL_SURFACE ( 'NONE', #11421, 1.500000000000001554 ) ;
#6529 = CARTESIAN_POINT ( 'NONE',  ( -29.21749237908258223, -82.58968536893642920, 17.32050807568881368 ) ) ;
#6530 = AXIS2_PLACEMENT_3D ( 'NONE', #17497, #5743, #53 ) ;
#6532 = EDGE_LOOP ( 'NONE', ( #8546, #12257, #8881, #16343 ) ) ;
#6531 = CARTESIAN_POINT ( 'NONE',  ( -18.39294862037050393, -23.16724548487935564, -8.660254037844380193 ) ) ;
#6533 = EDGE_CURVE ( 'NONE', #9368, #1680, #11667, .T. ) ;
#6534 = VERTEX_POINT ( 'NONE', #5321 ) ;
#6535 = ADVANCED_FACE ( 'NONE', ( #18351 ), #15074, .F. ) ;
#6536 = CARTESIAN_POINT ( 'NONE',  ( -70.00000000000000000, 44.99999999999999289, 25.00000000000000000 ) ) ;
#6537 = ORIENTED_EDGE ( 'NONE', *, *, #14509, .F. ) ;
#6538 = EDGE_LOOP ( 'NONE', ( #16683, #18334 ) ) ;
#6539 = AXIS2_PLACEMENT_3D ( 'NONE', #16797, #15339, #11824 ) ;
#6540 = DIRECTION ( 'NONE',  ( -1.000000000000000000, 0.000000000000000000, 0.000000000000000000 ) ) ;
#6541 = ORIENTED_EDGE ( 'NONE', *, *, #4930, .T. ) ;
#6542 = CARTESIAN_POINT ( 'NONE',  ( -25.76070822534488869, -82.04137586284720385, -8.660254037844385522 ) ) ;
#6543 = AXIS2_PLACEMENT_3D ( 'NONE', #896, #6679, #10996 ) ;
#6544 = CARTESIAN_POINT ( 'NONE',  ( -129.0548615328497704, 8.973171863034172802, -4.764204982952881196 ) ) ;
#6545 = CARTESIAN_POINT ( 'NONE',  ( -24.27922930231443743, -81.80638607452326028, 1.424741226644455312E-14 ) ) ;
#6546 = CARTESIAN_POINT ( 'NONE',  ( -46.50141314777110324, -85.33123289938248490, 12.99038105676661203 ) ) ;
#6547 = DIRECTION ( 'NONE',  ( -0.9876526153536336894, -0.1566598588826349503, 0.000000000000000000 ) ) ;
#6548 = DIRECTION ( 'NONE',  ( -0.1566598588826321747, 0.9876526153536343555, 0.000000000000000000 ) ) ;
#6549 = CARTESIAN_POINT ( 'NONE',  ( -58.68235252892885256, -24.49537676341649117, 17.32050807568882078 ) ) ;
#6550 = CARTESIAN_POINT ( 'NONE',  ( -24.81269062016911064, -24.18553456761645393, 1.869203119972154228E-14 ) ) ;
#6551 = ORIENTED_EDGE ( 'NONE', *, *, #17754, .F. ) ;
#6552 = FACE_BOUND ( 'NONE', #6375, .T. ) ;
#6553 = DIRECTION ( 'NONE',  ( -0.1566598588826321192, 0.9876526153536342445, 7.798540720466731404E-17 ) ) ;
#6554 = PLANE ( 'NONE',  #12638 ) ;
#6555 = AXIS2_PLACEMENT_3D ( 'NONE', #9212, #15463, #9693 ) ;
#6556 = DIRECTION ( 'NONE',  ( -0.9876526153536341335, -0.1566598588826327021, 0.000000000000000000 ) ) ;
#6557 = ADVANCED_FACE ( 'NONE', ( #2481, #16713, #2276 ), #3690, .T. ) ;
#6558 = DIRECTION ( 'NONE',  ( -0.000000000000000000, -0.000000000000000000, -1.000000000000000000 ) ) ;
#6559 = CIRCLE ( 'NONE', #17150, 20.00000000000001066 ) ;
#6560 = ORIENTED_EDGE ( 'NONE', *, *, #12128, .T. ) ;
#6561 = ORIENTED_EDGE ( 'NONE', *, *, #15989, .F. ) ;
#6562 = VERTEX_POINT ( 'NONE', #8269 ) ;
#6563 = CARTESIAN_POINT ( 'NONE',  ( -21.81009776393036503, -81.41473642731668292, 4.330127018922213189 ) ) ;
#6564 = ADVANCED_FACE ( 'NONE', ( #12589 ), #14031, .F. ) ;
#6565 = FACE_BOUND ( 'NONE', #8257, .T. ) ;
#6566 = AXIS2_PLACEMENT_3D ( 'NONE', #9723, #8725, #4274 ) ;
#6567 = SURFACE_STYLE_USAGE ( .BOTH. , #13734 ) ;
#6568 = ORIENTED_EDGE ( 'NONE', *, *, #8887, .T. ) ;
#6569 = CARTESIAN_POINT ( 'NONE',  ( -53.90880776292332399, -86.50618184100223118, 17.32050807568881368 ) ) ;
#6570 = DIRECTION ( 'NONE',  ( -0.1566598588826321192, 0.9876526153536342445, 7.798540720466730171E-17 ) ) ;
#6571 = AXIS2_PLACEMENT_3D ( 'NONE', #7564, #361, #10301 ) ;
#6572 = CARTESIAN_POINT ( 'NONE',  ( -36.46016868347218320, -20.97052993855726655, -12.99038105676658006 ) ) ;
#6573 = CARTESIAN_POINT ( 'NONE',  ( -67.57122606711152457, -25.90531549336017747, 21.65063509461101887 ) ) ;
#6574 = ORIENTED_EDGE ( 'NONE', *, *, #17615, .T. ) ;
#6575 = VERTEX_POINT ( 'NONE', #7885 ) ;
#6576 = DIRECTION ( 'NONE',  ( -0.1566598588826321192, 0.9876526153536342445, 7.798540720466730171E-17 ) ) ;
#6577 = AXIS2_PLACEMENT_3D ( 'NONE', #14959, #4445, #4637 ) ;
#6578 = CARTESIAN_POINT ( 'NONE',  ( -169.7775681651189359, 31.94775928504250828, -3.566331213966874802 ) ) ;
#6579 = ORIENTED_EDGE ( 'NONE', *, *, #14835, .F. ) ;
#6580 = EDGE_LOOP ( 'NONE', ( #2486, #233 ) ) ;
#6581 = DIRECTION ( 'NONE',  ( -0.1566598588826321747, 0.9876526153536343555, 0.000000000000000000 ) ) ;
#6582 = EDGE_CURVE ( 'NONE', #3440, #11862, #3867, .T. ) ;
#6583 = ORIENTED_EDGE ( 'NONE', *, *, #10801, .F. ) ;
#6584 = CIRCLE ( 'NONE', #13802, 144.0000000000000284 ) ;
#6585 = ORIENTED_EDGE ( 'NONE', *, *, #3981, .T. ) ;
#6586 = CARTESIAN_POINT ( 'NONE',  ( -129.0020721423141197, -14.74628763068006876, 4.579216830445306030 ) ) ;
#6587 = AXIS2_PLACEMENT_3D ( 'NONE', #16201, #17830, #10320 ) ;
#6588 = DIRECTION ( 'NONE',  ( -0.1566598588826321747, 0.9876526153536343555, 0.000000000000000000 ) ) ;
#6589 = ORIENTED_EDGE ( 'NONE', *, *, #6732, .F. ) ;
#6590 = ADVANCED_FACE ( 'NONE', ( #9580 ), #6759, .F. ) ;
#6591 = CARTESIAN_POINT ( 'NONE',  ( -3.373806069125576901, -15.72242466598909871, -12.99038105676658361 ) ) ;
#6592 = DIRECTION ( 'NONE',  ( -0.9876526153536341335, -0.1566598588826327021, 0.000000000000000000 ) ) ;
#6593 = APPLICATION_PROTOCOL_DEFINITION ( 'draft international standard', 'automotive_design', 1998, #12312 ) ;
#6594 = DIRECTION ( 'NONE',  ( -0.9876526153536344665, -0.1566598588826304539, 0.000000000000000000 ) ) ;
#6595 = LINE ( 'NONE', #1106, #10782 ) ;
#6596 = AXIS2_PLACEMENT_3D ( 'NONE', #2500, #798, #2210 ) ;
#6597 = LINE ( 'NONE', #18198, #9841 ) ;
#6598 = ORIENTED_EDGE ( 'NONE', *, *, #5915, .F. ) ;
#6599 = ORIENTED_EDGE ( 'NONE', *, *, #3449, .T. ) ;
#6600 = DIRECTION ( 'NONE',  ( -0.1566598588826321192, 0.9876526153536342445, 7.798540720466730171E-17 ) ) ;
#6601 = ORIENTED_EDGE ( 'NONE', *, *, #12754, .T. ) ;
#6602 = AXIS2_PLACEMENT_3D ( 'NONE', #5080, #17825, #13421 ) ;
#6603 = CYLINDRICAL_SURFACE ( 'NONE', #3323, 1.500000000000001554 ) ;
#6604 = VERTEX_POINT ( 'NONE', #2191 ) ;
#6605 = VERTEX_POINT ( 'NONE', #13729 ) ;
#6606 = DIRECTION ( 'NONE',  ( -0.1566598588826321192, 0.9876526153536342445, 7.798540720466731404E-17 ) ) ;
#6607 = CARTESIAN_POINT ( 'NONE',  ( -10.94591899504043830, -79.69147797960773971, -8.660254037844385522 ) ) ;
#6608 = ADVANCED_FACE ( 'NONE', ( #6477 ), #11174, .T. ) ;
#6609 = CIRCLE ( 'NONE', #9961, 1.500000000000000444 ) ;
#6610 = ADVANCED_FACE ( 'NONE', ( #13833 ), #10982, .F. ) ;
#6611 = CARTESIAN_POINT ( 'NONE',  ( -51.43967622453926936, -86.11453219379562540, -12.99038105676658539 ) ) ;
#6612 = AXIS2_PLACEMENT_3D ( 'NONE', #5503, #8254, #6833 ) ;
#6613 = ADVANCED_FACE ( 'NONE', ( #18051 ), #5122, .F. ) ;
#6614 = ORIENTED_EDGE ( 'NONE', *, *, #5686, .T. ) ;
#6615 = FACE_OUTER_BOUND ( 'NONE', #4732, .T. ) ;
#6616 = LINE ( 'NONE', #16563, #11182 ) ;
#6617 = CYLINDRICAL_SURFACE ( 'NONE', #15506, 1.500000000000001554 ) ;
#6618 = CARTESIAN_POINT ( 'NONE',  ( -33.20773785067495254, -25.51714336811882688, -8.660254037844380193 ) ) ;
#6620 = LINE ( 'NONE', #13700, #18712 ) ;
#6619 = AXIS2_PLACEMENT_3D ( 'NONE', #1307, #4209, #7090 ) ;
#6621 = CIRCLE ( 'NONE', #13250, 1.500000000000000888 ) ;
#6622 = FACE_OUTER_BOUND ( 'NONE', #6532, .T. ) ;
#6623 = VERTEX_POINT ( 'NONE', #3593 ) ;
#6624 = DIRECTION ( 'NONE',  ( 0.000000000000000000, 0.000000000000000000, 1.000000000000000000 ) ) ;
#6625 = AXIS2_PLACEMENT_3D ( 'NONE', #6206, #11932, #17783 ) ;
#6627 = EDGE_LOOP ( 'NONE', ( #13443, #6715 ) ) ;
#6626 = DIRECTION ( 'NONE',  ( 0.000000000000000000, 0.000000000000000000, 1.000000000000000000 ) ) ;
#6628 = CIRCLE ( 'NONE', #15992, 2.000000000000001776 ) ;
#6629 = CARTESIAN_POINT ( 'NONE',  ( -137.7298645655810390, -88.63485219053825404, -2.500000000000000000 ) ) ;
#6630 = ORIENTED_EDGE ( 'NONE', *, *, #13694, .F. ) ;
#6631 = VERTEX_POINT ( 'NONE', #5013 ) ;
#6632 = AXIS2_PLACEMENT_3D ( 'NONE', #16816, #17005, #15363 ) ;
#6633 = EDGE_CURVE ( 'NONE', #6767, #10467, #12583, .T. ) ;
#6634 = AXIS2_PLACEMENT_3D ( 'NONE', #15647, #121, #5899 ) ;
#6635 = CARTESIAN_POINT ( 'NONE',  ( 0.000000000000000000, 0.000000000000000000, -25.65685424949237614 ) ) ;
#6636 = EDGE_LOOP ( 'NONE', ( #4947, #17880 ) ) ;
#6637 = AXIS2_PLACEMENT_3D ( 'NONE', #15449, #17164, #1253 ) ;
#6638 = EDGE_CURVE ( 'NONE', #14394, #18427, #16605, .T. ) ;
#6639 = DIRECTION ( 'NONE',  ( 1.000000000000000000, 0.000000000000000000, -2.995206001686573514E-16 ) ) ;
#6640 = AXIS2_PLACEMENT_3D ( 'NONE', #4435, #5800, #15911 ) ;
#6641 = CARTESIAN_POINT ( 'NONE',  ( -52.96079015774756016, -28.65034054577145994, 8.660254037844417496 ) ) ;
#6642 = DIRECTION ( 'NONE',  ( -0.1566598588826321192, 0.9876526153536342445, 7.798540720466730171E-17 ) ) ;
#6643 = CARTESIAN_POINT ( 'NONE',  ( -11.76885329963143079, -17.05403346649147878, 4.330127018922214965 ) ) ;
#6644 = EDGE_CURVE ( 'NONE', #16906, #584, #12510, .T. ) ;
#6645 = CARTESIAN_POINT ( 'NONE',  ( 6.338001773648100468, -76.94993044916168401, 4.330127018922207860 ) ) ;
#6646 = CYLINDRICAL_SURFACE ( 'NONE', #2889, 1.500000000000001554 ) ;
#6647 = ORIENTED_EDGE ( 'NONE', *, *, #7816, .T. ) ;
#6648 = CARTESIAN_POINT ( 'NONE',  ( -25.80034323552273179, -24.34219442649909126, -4.330127018922181215 ) ) ;
#6649 = ORIENTED_EDGE ( 'NONE', *, *, #15138, .T. ) ;
#6650 = AXIS2_PLACEMENT_3D ( 'NONE', #8660, #1462, #13100 ) ;
#6651 = DIRECTION ( 'NONE',  ( 0.1856185419698760941, -0.9826218788918640312, 0.000000000000000000 ) ) ;
#6652 = CARTESIAN_POINT ( 'NONE',  ( -60.32854976272193426, -87.52447092373932946, 1.424741226644455312E-14 ) ) ;
#6653 = CIRCLE ( 'NONE', #5112, 1.500000000000000888 ) ;
#6654 = CIRCLE ( 'NONE', #10849, 1.500000000000000888 ) ;
#6655 = DIRECTION ( 'NONE',  ( -0.1566598588826321192, 0.9876526153536342445, 7.798540720466730171E-17 ) ) ;
#6656 = VECTOR ( 'NONE', #1400, 1000.000000000000114 ) ;
#6657 = AXIS2_PLACEMENT_3D ( 'NONE', #10017, #11248, #9918 ) ;
#6658 = EDGE_LOOP ( 'NONE', ( #18381, #17098, #18280, #11727 ) ) ;
#6659 = ORIENTED_EDGE ( 'NONE', *, *, #7525, .T. ) ;
#6660 = ORIENTED_EDGE ( 'NONE', *, *, #14355, .F. ) ;
#6661 = CARTESIAN_POINT ( 'NONE',  ( -61.15148406731293562, -24.88702641062305432, -21.65063509461097979 ) ) ;
#6662 = DIRECTION ( 'NONE',  ( -0.1566598588826321192, 0.9876526153536342445, 7.798540720466730171E-17 ) ) ;
#6663 = FACE_BOUND ( 'NONE', #6173, .T. ) ;
#6664 = CIRCLE ( 'NONE', #13904, 1.500000000000000444 ) ;
#6665 = CIRCLE ( 'NONE', #5763, 1.500000000000000000 ) ;
#6666 =( NAMED_UNIT ( * ) SI_UNIT ( $, .STERADIAN. ) SOLID_ANGLE_UNIT ( ) );
#6667 = AXIS2_PLACEMENT_3D ( 'NONE', #2385, #15368, #8179 ) ;
#6668 = ORIENTED_EDGE ( 'NONE', *, *, #8015, .T. ) ;
#6669 = EDGE_CURVE ( 'NONE', #7437, #4036, #13199, .T. ) ;
#6670 = AXIS2_PLACEMENT_3D ( 'NONE', #16259, #6506, #1856 ) ;
#6671 = ADVANCED_FACE ( 'NONE', ( #5609 ), #14507, .F. ) ;
#6672 = AXIS2_PLACEMENT_3D ( 'NONE', #10000, #8599, #16794 ) ;
#6673 = DIRECTION ( 'NONE',  ( -0.9876526153536336894, -0.1566598588826349503, 0.000000000000000000 ) ) ;
#6674 = EDGE_CURVE ( 'NONE', #7247, #8478, #1420, .T. ) ;
#6675 = DIRECTION ( 'NONE',  ( -0.1566598588826321747, 0.9876526153536343555, 0.000000000000000000 ) ) ;
#6676 = DIRECTION ( 'NONE',  ( -0.3915338189555022108, -0.9201637183752248150, 0.000000000000000000 ) ) ;
#6677 = LINE ( 'NONE', #18461, #4498 ) ;
#6678 = AXIS2_PLACEMENT_3D ( 'NONE', #16668, #13889, #938 ) ;
#6679 = DIRECTION ( 'NONE',  ( -0.1566598588826321747, 0.9876526153536343555, 0.000000000000000000 ) ) ;
#6680 = ORIENTED_EDGE ( 'NONE', *, *, #13245, .F. ) ;
#6681 = ORIENTED_EDGE ( 'NONE', *, *, #14864, .F. ) ;
#6682 = CARTESIAN_POINT ( 'NONE',  ( -79.23462711737164454, 33.01666666666666572, 35.00000000000000000 ) ) ;
#6683 = DIRECTION ( 'NONE',  ( 0.000000000000000000, -1.000000000000000000, 0.000000000000000000 ) ) ;
#6684 = AXIS2_PLACEMENT_3D ( 'NONE', #13513, #1968, #6353 ) ;
#6685 = LINE ( 'NONE', #8077, #535 ) ;
#6686 = VERTEX_POINT ( 'NONE', #4269 ) ;
#6687 = VERTEX_POINT ( 'NONE', #11275 ) ;
#6688 = CIRCLE ( 'NONE', #5783, 1.500000000000000000 ) ;
#6689 = DIRECTION ( 'NONE',  ( 0.000000000000000000, 0.000000000000000000, 1.000000000000000000 ) ) ;
#6690 = AXIS2_PLACEMENT_3D ( 'NONE', #577, #13809, #9474 ) ;
#6691 = ORIENTED_EDGE ( 'NONE', *, *, #4340, .T. ) ;
#6692 = CARTESIAN_POINT ( 'NONE',  ( -129.1404785418517918, -14.35070196317933444, 5.500000000000000000 ) ) ;
#6693 = CIRCLE ( 'NONE', #14262, 1.499999999999999556 ) ;
#6694 = DIRECTION ( 'NONE',  ( -0.1566598588826321192, 0.9876526153536342445, 7.798540720466731404E-17 ) ) ;
#6695 = AXIS2_PLACEMENT_3D ( 'NONE', #1408, #17348, #1501 ) ;
#6696 = CARTESIAN_POINT ( 'NONE',  ( -74.01821019817211322, 46.70976659135642706, 2.532235937273572546 ) ) ;
#6697 = DIRECTION ( 'NONE',  ( -2.289834988289385858E-16, 2.515349040166370903E-17, 1.000000000000000000 ) ) ;
#6698 = EDGE_CURVE ( 'NONE', #1785, #11499, #4062, .T. ) ;
#6699 = CARTESIAN_POINT ( 'NONE',  ( -85.13801595139509004, -33.83333333333328596, 29.99999999999997158 ) ) ;
#6700 = VECTOR ( 'NONE', #8705, 1000.000000000000000 ) ;
#6701 = CARTESIAN_POINT ( 'NONE',  ( -61.15148406731293562, -24.88702641062306498, 4.330127018922218518 ) ) ;
#6702 = DIRECTION ( 'NONE',  ( -0.000000000000000000, -0.000000000000000000, -1.000000000000000000 ) ) ;
#6703 = CIRCLE ( 'NONE', #4557, 1.500000000000000444 ) ;
#6704 = CARTESIAN_POINT ( 'NONE',  ( -26.78799585087635649, -24.49885428538171794, 1.887572821959364500E-14 ) ) ;
#6705 = ORIENTED_EDGE ( 'NONE', *, *, #18448, .F. ) ;
#6706 = EDGE_LOOP ( 'NONE', ( #11537, #8793, #17565, #15143, #11711, #8332 ) ) ;
#6707 = CARTESIAN_POINT ( 'NONE',  ( -65.10209452872746283, -25.51366584615358235, -17.32050807568878170 ) ) ;
#6708 = LINE ( 'NONE', #1115, #15776 ) ;
#6709 = EDGE_CURVE ( 'NONE', #495, #11172, #3514, .T. ) ;
#6710 = CIRCLE ( 'NONE', #12426, 1.500000000000001332 ) ;
#6711 = EDGE_LOOP ( 'NONE', ( #15884, #14174, #13431, #9586 ) ) ;
#6712 = DIRECTION ( 'NONE',  ( -0.000000000000000000, -0.000000000000000000, -1.000000000000000000 ) ) ;
#6713 = ORIENTED_EDGE ( 'NONE', *, *, #9464, .F. ) ;
#6714 = CIRCLE ( 'NONE', #11515, 1.500000000000000888 ) ;
#6715 = ORIENTED_EDGE ( 'NONE', *, *, #17929, .T. ) ;
#6716 = CARTESIAN_POINT ( 'NONE',  ( 1.399738696879940791, -77.73322974357483872, -12.99038105676658539 ) ) ;
#6717 = DIRECTION ( 'NONE',  ( -0.1566598588826321192, 0.9876526153536342445, 7.798540720466730171E-17 ) ) ;
#6718 = VECTOR ( 'NONE', #3890, 1000.000000000000000 ) ;
#6719 = DIRECTION ( 'NONE',  ( -0.1566598588826321192, 0.9876526153536342445, 7.798540720466730171E-17 ) ) ;
#6720 = FACE_OUTER_BOUND ( 'NONE', #17156, .T. ) ;
#6721 = DIRECTION ( 'NONE',  ( 0.000000000000000000, 0.000000000000000000, -1.000000000000000000 ) ) ;
#6722 = EDGE_LOOP ( 'NONE', ( #8948, #18422, #3755, #12459 ) ) ;
#6723 = DIRECTION ( 'NONE',  ( -0.9876526153536336894, -0.1566598588826349503, 0.000000000000000000 ) ) ;
#6724 = CIRCLE ( 'NONE', #5817, 1.500000000000000888 ) ;
#6725 = VECTOR ( 'NONE', #4576, 1000.000000000000000 ) ;
#6726 = DIRECTION ( 'NONE',  ( -0.1566598588826321192, 0.9876526153536342445, 7.798540720466730171E-17 ) ) ;
#6727 = CARTESIAN_POINT ( 'NONE',  ( -1.109027851681966492, -20.42569795443330349, 4.330127018922212301 ) ) ;
#6728 = CARTESIAN_POINT ( 'NONE',  ( -131.1404785418517918, -2.850701963179328668, 9.951701414186818625E-16 ) ) ;
#6729 = CARTESIAN_POINT ( 'NONE',  ( -312.1404785418517918, -2.850701963179328668, 9.951701414186818625E-16 ) ) ;
#6730 = ADVANCED_FACE ( 'NONE', ( #17288 ), #10046, .F. ) ;
#6731 = VERTEX_POINT ( 'NONE', #5807 ) ;
#6732 = EDGE_CURVE ( 'NONE', #15023, #17089, #2731, .T. ) ;
#6733 = CARTESIAN_POINT ( 'NONE',  ( -33.20773785067495965, -25.51714336811882688, 8.660254037844417496 ) ) ;
#6734 = ORIENTED_EDGE ( 'NONE', *, *, #17995, .T. ) ;
#6735 = EDGE_LOOP ( 'NONE', ( #1810, #13339, #14482, #10597 ) ) ;
#6736 = CIRCLE ( 'NONE', #4598, 1.500000000000000888 ) ;
#6737 = DIRECTION ( 'NONE',  ( 1.000000000000000000, 0.000000000000000000, 0.000000000000000000 ) ) ;
#6738 = ORIENTED_EDGE ( 'NONE', *, *, #9657, .F. ) ;
#6739 = SHAPE_REPRESENTATION ( 'Heavy-Duty Perforated Sieve Plate', ( #18772 ), #7243 ) ;
#6740 = VECTOR ( 'NONE', #9545, 1000.000000000000227 ) ;
#6741 = CARTESIAN_POINT ( 'NONE',  ( -13.45468554360235203, -22.38394619046619383, 17.32050807568881012 ) ) ;
#6742 = CARTESIAN_POINT ( 'NONE',  ( 5.350349158294472218, -77.10659030804430358, -8.660254037844389075 ) ) ;
#6743 = DIRECTION ( 'NONE',  ( -0.1566598588826321192, 0.9876526153536342445, 7.798540720466730171E-17 ) ) ;
#6744 = DIRECTION ( 'NONE',  ( -1.000000000000000000, 0.000000000000000000, 0.000000000000000000 ) ) ;
#6745 = DIRECTION ( 'NONE',  ( 1.000000000000000000, -3.469446951953611033E-15, 0.000000000000000000 ) ) ;
#6746 = EDGE_CURVE ( 'NONE', #12053, #8550, #16559, .T. ) ;
#6747 = EDGE_CURVE ( 'NONE', #592, #10493, #7480, .T. ) ;
#6748 = CARTESIAN_POINT ( 'NONE',  ( 0.3724510713484854851, -20.19070816610934926, -4.330127018922184767 ) ) ;
#6749 = CARTESIAN_POINT ( 'NONE',  ( -70.00000000000000000, 44.99999999999999289, 110.7545852194966045 ) ) ;
#6750 = ADVANCED_FACE ( 'NONE', ( #1268 ), #17183, .F. ) ;
#6751 = CYLINDRICAL_SURFACE ( 'NONE', #8086, 1.500000000000001554 ) ;
#6752 = DIRECTION ( 'NONE',  ( -0.1566598588826321192, 0.9876526153536342445, 7.798540720466731404E-17 ) ) ;
#6753 = DIRECTION ( 'NONE',  ( 0.000000000000000000, 0.000000000000000000, 1.000000000000000000 ) ) ;
#6754 = VECTOR ( 'NONE', #18264, 1000.000000000000000 ) ;
#6755 = AXIS2_PLACEMENT_3D ( 'NONE', #18070, #9797, #5035 ) ;
#6756 = VERTEX_POINT ( 'NONE', #7228 ) ;
#6757 = ORIENTED_EDGE ( 'NONE', *, *, #2364, .T. ) ;
#6758 = ORIENTED_EDGE ( 'NONE', *, *, #12819, .F. ) ;
#6759 = CYLINDRICAL_SURFACE ( 'NONE', #12888, 1.500000000000001554 ) ;
#6760 = FACE_BOUND ( 'NONE', #13461, .T. ) ;
#6761 = CARTESIAN_POINT ( 'NONE',  ( -62.30385499342917655, -87.83779064150458282, 17.32050807568881368 ) ) ;
#6762 = ORIENTED_EDGE ( 'NONE', *, *, #15332, .T. ) ;
#6763 = CARTESIAN_POINT ( 'NONE',  ( 2.447859171744382056, -14.79900155049411659, 30.00000000000000000 ) ) ;
#6764 = AXIS2_PLACEMENT_3D ( 'NONE', #18128, #1152, #8252 ) ;
#6765 = DIRECTION ( 'NONE',  ( -0.9876526153536341335, -0.1566598588826327021, 0.000000000000000000 ) ) ;
#6766 = DIRECTION ( 'NONE',  ( -0.1566598588826321192, 0.9876526153536342445, 7.798540720466731404E-17 ) ) ;
#6767 = VERTEX_POINT ( 'NONE', #2765 ) ;
#6768 = DIRECTION ( 'NONE',  ( 0.000000000000000000, 0.000000000000000000, 1.000000000000000000 ) ) ;
#6769 = CARTESIAN_POINT ( 'NONE',  ( -68.76323200340563346, -31.15689828789355786, -4.330127018922181215 ) ) ;
#6770 = ORIENTED_EDGE ( 'NONE', *, *, #16936, .F. ) ;
#6771 = CARTESIAN_POINT ( 'NONE',  ( -89.99999999999998579, -35.00000000000001421, 2.500000000000000000 ) ) ;
#6772 = DIRECTION ( 'NONE',  ( -0.9539392014169452150, 0.3000000000000013212, -0.000000000000000000 ) ) ;
#6773 = ORIENTED_EDGE ( 'NONE', *, *, #8841, .F. ) ;
#6774 = DIRECTION ( 'NONE',  ( -0.1566598588826321747, 0.9876526153536343555, 0.000000000000000000 ) ) ;
#6775 = VERTEX_POINT ( 'NONE', #5704 ) ;
#6776 = EDGE_CURVE ( 'NONE', #6575, #10405, #15327, .T. ) ;
#6777 = CARTESIAN_POINT ( 'NONE',  ( -49.59961335071796640, 37.20051552679456108, -20.00000000000000355 ) ) ;
#6778 = EDGE_LOOP ( 'NONE', ( #608, #18440 ) ) ;
#6779 = ORIENTED_EDGE ( 'NONE', *, *, #9879, .F. ) ;
#6780 = ORIENTED_EDGE ( 'NONE', *, *, #3079, .F. ) ;
#6781 = DIRECTION ( 'NONE',  ( -0.9876526153536336894, -0.1566598588826349503, 0.000000000000000000 ) ) ;
#6782 = EDGE_CURVE ( 'NONE', #18003, #9146, #2917, .T. ) ;
#6783 = ORIENTED_EDGE ( 'NONE', *, *, #8007, .F. ) ;
#6784 = ORIENTED_EDGE ( 'NONE', *, *, #9685, .T. ) ;
#6785 = CARTESIAN_POINT ( 'NONE',  ( -50.49165861936347710, -28.25869089856488614, -4.330127018922181215 ) ) ;
#6786 = DIRECTION ( 'NONE',  ( -0.1566598588826321192, 0.9876526153536342445, 7.798540720466730171E-17 ) ) ;
#6787 = CARTESIAN_POINT ( 'NONE',  ( -27.73601345605213098, -82.35469558061248563, 8.660254037844412167 ) ) ;
#6788 = ORIENTED_EDGE ( 'NONE', *, *, #7078, .F. ) ;
#6789 = AXIS2_PLACEMENT_3D ( 'NONE', #1128, #4024, #11317 ) ;
#6790 = FACE_OUTER_BOUND ( 'NONE', #3008, .T. ) ;
#6791 = DIRECTION ( 'NONE',  ( -0.1566598588826321192, 0.9876526153536342445, 7.798540720466730171E-17 ) ) ;
#6792 = EDGE_LOOP ( 'NONE', ( #15256, #13335, #18274, #11790 ) ) ;
#6793 = CARTESIAN_POINT ( 'NONE',  ( -79.24244631363546887, 32.81909429640987952, 35.00000000000000000 ) ) ;
#6794 = CARTESIAN_POINT ( 'NONE',  ( -9.299721761247353058, -16.66238381928489787, -8.660254037844380193 ) ) ;
#6795 = VERTEX_POINT ( 'NONE', #8722 ) ;
#6796 = ORIENTED_EDGE ( 'NONE', *, *, #3719, .T. ) ;
#6797 = CARTESIAN_POINT ( 'NONE',  ( 5.481473465377021625, 12.88229205725314763, -25.00000000000000000 ) ) ;
#6798 = CARTESIAN_POINT ( 'NONE',  ( -77.18258565727083464, 4.450738551673830479, -130.3485206753969976 ) ) ;
#6799 = EDGE_LOOP ( 'NONE', ( #14200, #3844 ) ) ;
#6800 = EDGE_LOOP ( 'NONE', ( #16950, #8358, #3919, #2842 ) ) ;
#6801 = VERTEX_POINT ( 'NONE', #8350 ) ;
#6802 = EDGE_CURVE ( 'NONE', #18385, #13575, #10178, .T. ) ;
#6803 = DIRECTION ( 'NONE',  ( -0.9876526153536336894, -0.1566598588826349503, 0.000000000000000000 ) ) ;
#6804 = ORIENTED_EDGE ( 'NONE', *, *, #2884, .F. ) ;
#6805 = ORIENTED_EDGE ( 'NONE', *, *, #945, .F. ) ;
#6806 = DIRECTION ( 'NONE',  ( -0.1566598588826321192, 0.9876526153536342445, 7.798540720466730171E-17 ) ) ;
#6807 = EDGE_CURVE ( 'NONE', #8991, #4362, #4132, .T. ) ;
#6808 = DIRECTION ( 'NONE',  ( -0.1566598588826321192, 0.9876526153536342445, 7.798540720466731404E-17 ) ) ;
#6809 = ORIENTED_EDGE ( 'NONE', *, *, #5345, .T. ) ;
#6810 = DIRECTION ( 'NONE',  ( -0.1566598588826321747, 0.9876526153536343555, 0.000000000000000000 ) ) ;
#6811 = CARTESIAN_POINT ( 'NONE',  ( -1.069392841504132052, -78.12487939078141608, 8.660254037844408614 ) ) ;
#6812 = CARTESIAN_POINT ( 'NONE',  ( -33.99103714508810725, -20.57888029135068564, -17.32050807568878170 ) ) ;
#6813 = EDGE_CURVE ( 'NONE', #8885, #17191, #814, .T. ) ;
#6814 = CARTESIAN_POINT ( 'NONE',  ( -129.1404785418517918, -2.850701963179328668, 9.951701414186818625E-16 ) ) ;
#6815 = ORIENTED_EDGE ( 'NONE', *, *, #18720, .T. ) ;
#6816 = DIRECTION ( 'NONE',  ( -0.1566598588826321192, 0.9876526153536342445, 7.798540720466730171E-17 ) ) ;
#6817 = CARTESIAN_POINT ( 'NONE',  ( 0.000000000000000000, 0.000000000000000000, 35.00000000000000000 ) ) ;
#6818 = VERTEX_POINT ( 'NONE', #8449 ) ;
#6819 = DIRECTION ( 'NONE',  ( -0.1566598588826321192, 0.9876526153536342445, 7.798540720466731404E-17 ) ) ;
#6820 = CARTESIAN_POINT ( 'NONE',  ( -1.892327146095128310, -15.48743487766515337, -21.65063509461097979 ) ) ;
#6821 = ORIENTED_EDGE ( 'NONE', *, *, #16993, .F. ) ;
#6822 = EDGE_LOOP ( 'NONE', ( #11394, #15808, #4959, #12412, #9912, #4907, #14046, #6551, #3842, #17985 ) ) ;
#6823 = DIRECTION ( 'NONE',  ( -0.000000000000000000, -0.000000000000000000, -1.000000000000000000 ) ) ;
#6824 = AXIS2_PLACEMENT_3D ( 'NONE', #14696, #1715, #295 ) ;
#6825 = CARTESIAN_POINT ( 'NONE',  ( -61.15148406731292852, -24.88702641062306853, 12.99038105676661736 ) ) ;
#6826 = EDGE_LOOP ( 'NONE', ( #3695, #17374, #13877, #10071 ) ) ;
#6827 = ORIENTED_EDGE ( 'NONE', *, *, #15332, .F. ) ;
#6828 = EDGE_CURVE ( 'NONE', #7702, #4043, #15943, .T. ) ;
#6829 = DIRECTION ( 'NONE',  ( -0.000000000000000000, -0.000000000000000000, -1.000000000000000000 ) ) ;
#6830 = ORIENTED_EDGE ( 'NONE', *, *, #16402, .F. ) ;
#6831 = CARTESIAN_POINT ( 'NONE',  ( 0.5768043922889515285, -15.09578523045857601, 1.387778780781445676E-14 ) ) ;
#6832 = DIRECTION ( 'NONE',  ( -0.9876526153536336894, -0.1566598588826349503, 0.000000000000000000 ) ) ;
#6833 = DIRECTION ( 'NONE',  ( 0.000000000000000000, 0.000000000000000000, 1.000000000000000000 ) ) ;
#6834 = ADVANCED_FACE ( 'NONE', ( #278 ), #13432, .F. ) ;
#6835 = CARTESIAN_POINT ( 'NONE',  ( -74.48479437458692587, -27.00193450553859975, 12.99038105676661736 ) ) ;
#6836 = AXIS2_PLACEMENT_3D ( 'NONE', #4412, #4603, #1671 ) ;
#6837 = CARTESIAN_POINT ( 'NONE',  ( -128.0119535342735162, 9.482588595290904365, -3.146712427857100813 ) ) ;
#6838 = CARTESIAN_POINT ( 'NONE',  ( -24.11451099155181055, -19.01228170252437621, 1.908195823574487804E-14 ) ) ;
#6839 = DIRECTION ( 'NONE',  ( -0.1566598588826321192, 0.9876526153536342445, 7.798540720466730171E-17 ) ) ;
#6840 = CARTESIAN_POINT ( 'NONE',  ( 3.868870235264020963, -77.34158009636824715, 8.660254037844406838 ) ) ;
#6841 = DIRECTION ( 'NONE',  ( -0.1566598588826321192, 0.9876526153536342445, 7.798540720466730171E-17 ) ) ;
#6842 = DIRECTION ( 'NONE',  ( -0.1566598588826321747, 0.9876526153536343555, 0.000000000000000000 ) ) ;
#6843 = EDGE_CURVE ( 'NONE', #15127, #18093, #17788, .T. ) ;
#6844 = ORIENTED_EDGE ( 'NONE', *, *, #3876, .F. ) ;
#6845 = ORIENTED_EDGE ( 'NONE', *, *, #17437, .F. ) ;
#6846 = DIRECTION ( 'NONE',  ( -0.1566598588826321192, 0.9876526153536342445, 7.798540720466730171E-17 ) ) ;
#6847 = VECTOR ( 'NONE', #13289, 1000.000000000000000 ) ;
#6848 = FACE_BOUND ( 'NONE', #1003, .T. ) ;
#6849 = EDGE_CURVE ( 'NONE', #4027, #10083, #5028, .T. ) ;
#6850 = EDGE_CURVE ( 'NONE', #9530, #15072, #16018, .T. ) ;
#6851 = EDGE_CURVE ( 'NONE', #9656, #13932, #13209, .T. ) ;
#6852 = DIRECTION ( 'NONE',  ( -0.9876526153536336894, -0.1566598588826349503, 0.000000000000000000 ) ) ;
#6853 = ADVANCED_FACE ( 'NONE', ( #10324 ), #7681, .F. ) ;
#6854 = VECTOR ( 'NONE', #17010, 1000.000000000000000 ) ;
#6855 = LINE ( 'NONE', #15555, #2790 ) ;
#6856 = VERTEX_POINT ( 'NONE', #1891 ) ;
#6857 = EDGE_CURVE ( 'NONE', #3864, #11862, #1141, .T. ) ;
#6858 = CARTESIAN_POINT ( 'NONE',  ( -15.88418207180859021, -80.47477727402089442, 17.32050807568881368 ) ) ;
#6859 = CYLINDRICAL_SURFACE ( 'NONE', #14548, 1.500000000000001554 ) ;
#6860 = CIRCLE ( 'NONE', #12271, 1.500000000000000000 ) ;
#6861 = FACE_OUTER_BOUND ( 'NONE', #5941, .T. ) ;
#6862 = DIRECTION ( 'NONE',  ( -0.1566598588826321192, 0.9876526153536342445, 7.798540720466730171E-17 ) ) ;
#6863 = VERTEX_POINT ( 'NONE', #7588 ) ;
#6864 = DIRECTION ( 'NONE',  ( -0.1566598588826321192, 0.9876526153536342445, 7.798540720466731404E-17 ) ) ;
#6865 = DIRECTION ( 'NONE',  ( -0.1566598588826321192, 0.9876526153536342445, 7.798540720466731404E-17 ) ) ;
#6866 = ORIENTED_EDGE ( 'NONE', *, *, #10556, .T. ) ;
#6867 = ORIENTED_EDGE ( 'NONE', *, *, #149, .T. ) ;
#6868 = DIRECTION ( 'NONE',  ( -0.9876526153536336894, -0.1566598588826349503, 0.000000000000000000 ) ) ;
#6869 = AXIS2_PLACEMENT_3D ( 'NONE', #11921, #3408, #7701 ) ;
#6870 = ORIENTED_EDGE ( 'NONE', *, *, #12537, .F. ) ;
#6871 = VERTEX_POINT ( 'NONE', #14600 ) ;
#6872 = EDGE_LOOP ( 'NONE', ( #11162, #9996 ) ) ;
#6873 = DIRECTION ( 'NONE',  ( -0.1566598588826321747, 0.9876526153536343555, 0.000000000000000000 ) ) ;
#6874 = EDGE_CURVE ( 'NONE', #4290, #2224, #3384, .T. ) ;
#6875 = CARTESIAN_POINT ( 'NONE',  ( -31.68662391746666884, -82.98133501614299234, -21.65063509461098690 ) ) ;
#6876 = EDGE_CURVE ( 'NONE', #16997, #15396, #17665, .T. ) ;
#6877 = AXIS2_PLACEMENT_3D ( 'NONE', #15519, #2535, #8321 ) ;
#6878 = CARTESIAN_POINT ( 'NONE',  ( -25.59598991458226536, -19.24727149084832334, 1.908195823574487804E-14 ) ) ;
#6879 = EDGE_CURVE ( 'NONE', #10372, #16881, #9888, .T. ) ;
#6880 = ADVANCED_FACE ( 'NONE', ( #3289 ), #13354, .F. ) ;
#6881 = LINE ( 'NONE', #5445, #2705 ) ;
#6882 = DIRECTION ( 'NONE',  ( -0.000000000000000000, -0.000000000000000000, 1.000000000000000000 ) ) ;
#6883 = PRODUCT_CONTEXT ( 'NONE', #7500, 'mechanical' ) ;
#6884 = EDGE_CURVE ( 'NONE', #17521, #15703, #14735, .T. ) ;
#6885 = CARTESIAN_POINT ( 'NONE',  ( -44.07191661956487394, -27.24040181582776299, 21.65063509461101887 ) ) ;
#6886 = CARTESIAN_POINT ( 'NONE',  ( -10.94591899504043830, -79.69147797960773971, 17.32050807568880657 ) ) ;
#6887 = CARTESIAN_POINT ( 'NONE',  ( -62.63296299034337977, -25.12201619894701921, 21.65063509461101887 ) ) ;
#6888 = CARTESIAN_POINT ( 'NONE',  ( -42.38608437559395981, -21.91048909185305860, -17.32050807568878170 ) ) ;
#6889 = EDGE_LOOP ( 'NONE', ( #14349, #9083 ) ) ;
#6890 = ORIENTED_EDGE ( 'NONE', *, *, #2261, .F. ) ;
#6891 = CARTESIAN_POINT ( 'NONE',  ( -6.830590222863280658, -16.27073417207831696, -12.99038105676658006 ) ) ;
#6892 = DIRECTION ( 'NONE',  ( -0.1566598588826321192, 0.9876526153536342445, 7.798540720466730171E-17 ) ) ;
#6893 = CIRCLE ( 'NONE', #4441, 1.500000000000000888 ) ;
#6894 = VERTEX_POINT ( 'NONE', #8820 ) ;
#6895 = CIRCLE ( 'NONE', #12602, 1.500000000000000444 ) ;
#6896 = ORIENTED_EDGE ( 'NONE', *, *, #15184, .T. ) ;
#6897 = ORIENTED_EDGE ( 'NONE', *, *, #10465, .T. ) ;
#6898 = CIRCLE ( 'NONE', #6285, 1.500000000000000888 ) ;
#6899 = ORIENTED_EDGE ( 'NONE', *, *, #14075, .F. ) ;
#6900 = CARTESIAN_POINT ( 'NONE',  ( -60.36818477289978091, -29.82528948739120267, -4.330127018922181215 ) ) ;
#6901 = CIRCLE ( 'NONE', #207, 1.500000000000000000 ) ;
#6902 = FACE_OUTER_BOUND ( 'NONE', #9213, .T. ) ;
#6903 = EDGE_LOOP ( 'NONE', ( #14678, #731 ) ) ;
#6904 = CARTESIAN_POINT ( 'NONE',  ( -6.830590222863280658, -16.27073417207831696, -21.65063509461097979 ) ) ;
#6905 = CYLINDRICAL_SURFACE ( 'NONE', #8217, 1.500000000000001554 ) ;
#6906 = COLOUR_RGB ( '', 0.40784314, 0.44705882, 0.49803922) ;
#6907 = CYLINDRICAL_SURFACE ( 'NONE', #5528, 1.500000000000001554 ) ;
#6908 = EDGE_CURVE ( 'NONE', #10401, #2351, #9091, .T. ) ;
#6909 = CIRCLE ( 'NONE', #4156, 1.500000000000000888 ) ;
#6910 = EDGE_CURVE ( 'NONE', #13845, #9583, #3205, .T. ) ;
#6911 = CARTESIAN_POINT ( 'NONE',  ( 3.231158466157551423, 19.73726462726227737, 30.00000000000000000 ) ) ;
#6912 = VERTEX_POINT ( 'NONE', #17562 ) ;
#6913 = CARTESIAN_POINT ( 'NONE',  ( -5.842937607509656850, -16.11407431319567962, -8.660254037844383745 ) ) ;
#6914 = VECTOR ( 'NONE', #1138, 1000.000000000000000 ) ;
#6915 = DIRECTION ( 'NONE',  ( 0.000000000000000000, 0.000000000000000000, 1.000000000000000000 ) ) ;
#6916 = VERTEX_POINT ( 'NONE', #11903 ) ;
#6917 = ORIENTED_EDGE ( 'NONE', *, *, #14126, .F. ) ;
#6918 = LINE ( 'NONE', #8236, #935 ) ;
#6919 = EDGE_CURVE ( 'NONE', #7360, #8286, #5657, .T. ) ;
#6920 = CARTESIAN_POINT ( 'NONE',  ( -55.39028668595378946, -86.74117162932616054, 1.424741226644455312E-14 ) ) ;
#6921 = ORIENTED_EDGE ( 'NONE', *, *, #8263, .F. ) ;
#6922 = DIRECTION ( 'NONE',  ( -0.000000000000000000, -0.000000000000000000, -1.000000000000000000 ) ) ;
#6923 = ORIENTED_EDGE ( 'NONE', *, *, #10688, .F. ) ;
#6924 = CIRCLE ( 'NONE', #12948, 5.000000000000004441 ) ;
#6925 = CARTESIAN_POINT ( 'NONE',  ( -37.15834831208948685, -26.14378280364935137, 4.330127018922217630 ) ) ;
#6926 = ORIENTED_EDGE ( 'NONE', *, *, #11211, .T. ) ;
#6927 = CYLINDRICAL_SURFACE ( 'NONE', #2158, 2.000000000000000000 ) ;
#6928 = AXIS2_PLACEMENT_3D ( 'NONE', #3279, #2914, #16006 ) ;
#6929 = CARTESIAN_POINT ( 'NONE',  ( -16.70711637639958269, -17.83733276090463704, -12.99038105676658006 ) ) ;
#6930 = AXIS2_PLACEMENT_3D ( 'NONE', #1478, #10361, #14820 ) ;
#6931 = ORIENTED_EDGE ( 'NONE', *, *, #9658, .T. ) ;
#6932 = FACE_OUTER_BOUND ( 'NONE', #6792, .T. ) ;
#6933 = DIRECTION ( 'NONE',  ( -0.1566598588826321747, 0.9876526153536343555, 0.000000000000000000 ) ) ;
#6934 = TOROIDAL_SURFACE ( 'NONE', #9324, 12.83663829214476770, 3.000000000000000000 ) ;
#6935 = AXIS2_PLACEMENT_3D ( 'NONE', #14271, #13975, #11303 ) ;
#6936 = DIRECTION ( 'NONE',  ( 0.8007491221077702725, -0.5989998693185459855, 7.771473782954798134E-17 ) ) ;
#6937 = DIRECTION ( 'NONE',  ( -0.9876526153536341335, -0.1566598588826327021, 0.000000000000000000 ) ) ;
#6938 = LINE ( 'NONE', #3860, #5331 ) ;
#6939 =( GEOMETRIC_REPRESENTATION_CONTEXT ( 3 ) GLOBAL_UNCERTAINTY_ASSIGNED_CONTEXT ( ( #18038 ) ) GLOBAL_UNIT_ASSIGNED_CONTEXT ( ( #13334, #6156, #4703 ) ) REPRESENTATION_CONTEXT ( 'NONE', 'WORKASPACE' ) );
#6940 = FACE_OUTER_BOUND ( 'NONE', #17475, .T. ) ;
#6941 = LINE ( 'NONE', #15910, #8162 ) ;
#6942 = EDGE_CURVE ( 'NONE', #8675, #2583, #10475, .T. ) ;
#6943 = CARTESIAN_POINT ( 'NONE',  ( -81.87192997736541145, 3.395211045985502274, 2.500000000000000000 ) ) ;
#6944 = CARTESIAN_POINT ( 'NONE',  ( -90.00000000000000000, 34.99999999999999289, 35.00000000000000000 ) ) ;
#6945 = DIRECTION ( 'NONE',  ( -0.1566598588826321192, 0.9876526153536342445, 7.798540720466730171E-17 ) ) ;
#6946 = AXIS2_PLACEMENT_3D ( 'NONE', #7148, #8366, #8652 ) ;
#6947 = ORIENTED_EDGE ( 'NONE', *, *, #17202, .F. ) ;
#6948 = EDGE_CURVE ( 'NONE', #17749, #6040, #11965, .T. ) ;
#6949 = DIRECTION ( 'NONE',  ( 0.000000000000000000, 0.000000000000000000, 1.000000000000000000 ) ) ;
#6950 = AXIS2_PLACEMENT_3D ( 'NONE', #15037, #554, #3275 ) ;
#6951 = AXIS2_PLACEMENT_3D ( 'NONE', #11018, #15960, #17222 ) ;
#6952 = FACE_BOUND ( 'NONE', #1581, .T. ) ;
#6953 = AXIS2_PLACEMENT_3D ( 'NONE', #16028, #3038, #6955 ) ;
#6954 = AXIS2_PLACEMENT_3D ( 'NONE', #7988, #13847, #13749 ) ;
#6955 = DIRECTION ( 'NONE',  ( 1.000000000000000000, 0.000000000000000000, 0.000000000000000000 ) ) ;
#6956 = DIRECTION ( 'NONE',  ( 0.000000000000000000, 0.000000000000000000, 1.000000000000000000 ) ) ;
#6957 = ORIENTED_EDGE ( 'NONE', *, *, #7845, .F. ) ;
#6958 = FACE_BOUND ( 'NONE', #7399, .T. ) ;
#6959 = ORIENTED_EDGE ( 'NONE', *, *, #2803, .T. ) ;
#6960 = ORIENTED_EDGE ( 'NONE', *, *, #9156, .T. ) ;
#6961 = DIRECTION ( 'NONE',  ( -0.3000000000000046518, 0.9539392014169442158, 0.000000000000000000 ) ) ;
#6962 = CIRCLE ( 'NONE', #2093, 1.500000000000000000 ) ;
#6963 = AXIS2_PLACEMENT_3D ( 'NONE', #2897, #11424, #17257 ) ;
#6964 = CYLINDRICAL_SURFACE ( 'NONE', #1254, 1.500000000000001554 ) ;
#6965 = LINE ( 'NONE', #13949, #18478 ) ;
#6966 = EDGE_CURVE ( 'NONE', #495, #1369, #12745, .T. ) ;
#6967 = DIRECTION ( 'NONE',  ( 1.224646799147353207E-16, 1.000000000000000000, -0.000000000000000000 ) ) ;
#6968 = ADVANCED_FACE ( 'NONE', ( #5563 ), #11028, .F. ) ;
#6969 = ORIENTED_EDGE ( 'NONE', *, *, #14374, .F. ) ;
#6970 = EDGE_CURVE ( 'NONE', #7134, #7610, #18553, .T. ) ;
#6971 = ORIENTED_EDGE ( 'NONE', *, *, #14943, .T. ) ;
#6972 = AXIS2_PLACEMENT_3D ( 'NONE', #1695, #11808, #17736 ) ;
#6973 = ORIENTED_EDGE ( 'NONE', *, *, #1147, .F. ) ;
#6974 = CARTESIAN_POINT ( 'NONE',  ( -75.18297400320422241, -32.17518737063066681, -12.99038105676658006 ) ) ;
#6975 = EDGE_LOOP ( 'NONE', ( #16868, #17786, #13752 ) ) ;
#6976 = CARTESIAN_POINT ( 'NONE',  ( -18.39294862037050393, -23.16724548487935564, 17.32050807568881012 ) ) ;
#6977 = DIRECTION ( 'NONE',  ( -0.1566598588826321192, 0.9876526153536342445, 7.798540720466730171E-17 ) ) ;
#6978 = AXIS2_PLACEMENT_3D ( 'NONE', #10780, #5002, #16596 ) ;
#6979 = AXIS2_PLACEMENT_3D ( 'NONE', #8434, #14108, #1252 ) ;
#6980 = CARTESIAN_POINT ( 'NONE',  ( -18.35331361019266794, -80.86642692122747178, -21.65063509461098690 ) ) ;
#6981 = UNCERTAINTY_MEASURE_WITH_UNIT (LENGTH_MEASURE( 1.000000000000000082E-05 ), #18508, 'distance_accuracy_value', 'NONE');
#6982 = DIRECTION ( 'NONE',  ( -0.1566598588826321192, 0.9876526153536342445, 7.798540720466730171E-17 ) ) ;
#6983 = DIRECTION ( 'NONE',  ( 0.1856185419698755945, -0.9826218788918641422, 0.000000000000000000 ) ) ;
#6984 = CARTESIAN_POINT ( 'NONE',  ( -2.096680467035594297, -20.58235781331593017, 17.32050807568881012 ) ) ;
#6985 = PRODUCT_CONTEXT ( 'NONE', #9441, 'mechanical' ) ;
#6986 = AXIS2_PLACEMENT_3D ( 'NONE', #14877, #11908, #17753 ) ;
#6987 = EDGE_CURVE ( 'NONE', #4041, #405, #2524, .T. ) ;
#6988 = DIRECTION ( 'NONE',  ( 3.816390434826605238E-17, 0.000000000000000000, -1.000000000000000000 ) ) ;
#6990 = FACE_OUTER_BOUND ( 'NONE', #11626, .T. ) ;
#6989 = CIRCLE ( 'NONE', #9699, 1.500000000000000888 ) ;
#6991 = ADVANCED_FACE ( 'NONE', ( #4109 ), #15684, .F. ) ;
#6992 = DIRECTION ( 'NONE',  ( -0.1566598588826321747, 0.9876526153536343555, 0.000000000000000000 ) ) ;
#6993 = AXIS2_PLACEMENT_3D ( 'NONE', #998, #3879, #9706 ) ;
#6994 = EDGE_CURVE ( 'NONE', #10517, #13155, #1039, .T. ) ;
#6995 = EDGE_LOOP ( 'NONE', ( #3194, #1957 ) ) ;
#6996 = ORIENTED_EDGE ( 'NONE', *, *, #909, .F. ) ;
#6997 = FACE_BOUND ( 'NONE', #14198, .T. ) ;
#6998 = DIRECTION ( 'NONE',  ( -0.1566598588826321747, 0.9876526153536343555, 0.000000000000000000 ) ) ;
#6999 = ORIENTED_EDGE ( 'NONE', *, *, #5217, .T. ) ;
#7000 = CARTESIAN_POINT ( 'NONE',  ( 5.481473465377026955, -12.88229205725314763, 25.00000000000000000 ) ) ;
#7001 = EDGE_LOOP ( 'NONE', ( #5092, #10155, #5120 ) ) ;
#7002 = LINE ( 'NONE', #8396, #16381 ) ;
#7003 = CIRCLE ( 'NONE', #9985, 1.500000000000000888 ) ;
#7004 = AXIS2_PLACEMENT_3D ( 'NONE', #560, #17471, #2064 ) ;
#7005 = DIRECTION ( 'NONE',  ( -0.1566598588826321192, 0.9876526153536342445, 7.798540720466731404E-17 ) ) ;
#7006 = ORIENTED_EDGE ( 'NONE', *, *, #12572, .T. ) ;
#7007 = AXIS2_PLACEMENT_3D ( 'NONE', #17388, #7237, #5820 ) ;
#7008 = CARTESIAN_POINT ( 'NONE',  ( -129.1404785418517918, 8.737252551174764292, 5.316095106350545940 ) ) ;
#7009 = CARTESIAN_POINT ( 'NONE',  ( -105.1664215174088213, -37.48287248576487940, 2.500000000000000000 ) ) ;
#7010 = CIRCLE ( 'NONE', #17608, 1.500000000000000000 ) ;
#7011 = DIRECTION ( 'NONE',  ( -0.1566598588826321747, 0.9876526153536343555, 0.000000000000000000 ) ) ;
#7012 = AXIS2_PLACEMENT_3D ( 'NONE', #4591, #18680, #4404 ) ;
#7013 = LINE ( 'NONE', #6911, #16951 ) ;
#7014 = ORIENTED_EDGE ( 'NONE', *, *, #16058, .T. ) ;
#7015 = FACE_OUTER_BOUND ( 'NONE', #9447, .T. ) ;
#7016 = AXIS2_PLACEMENT_3D ( 'NONE', #6904, #12643, #18504 ) ;
#7017 = CARTESIAN_POINT ( 'NONE',  ( -71.90911978745813826, 1.387778780781445676E-14, -19.99999999999999645 ) ) ;
#7018 = CARTESIAN_POINT ( 'NONE',  ( -62.00000000000000000, 0.000000000000000000, -20.00000000000000000 ) ) ;
#7019 = ORIENTED_EDGE ( 'NONE', *, *, #12476, .F. ) ;
#7020 = CARTESIAN_POINT ( 'NONE',  ( -48.80582637539257718, -22.92877817459016043, -17.32050807568878170 ) ) ;
#7021 = DIRECTION ( 'NONE',  ( -0.1566598588826321747, 0.9876526153536343555, 0.000000000000000000 ) ) ;
#7022 = VERTEX_POINT ( 'NONE', #18303 ) ;
#7023 = DIRECTION ( 'NONE',  ( 0.000000000000000000, 0.000000000000000000, 1.000000000000000000 ) ) ;
#7024 = ORIENTED_EDGE ( 'NONE', *, *, #3448, .F. ) ;
#7025 = ORIENTED_EDGE ( 'NONE', *, *, #9830, .T. ) ;
#7026 = EDGE_CURVE ( 'NONE', #9621, #17252, #7002, .T. ) ;
#7027 = EDGE_CURVE ( 'NONE', #5678, #15183, #8312, .T. ) ;
#7028 = CARTESIAN_POINT ( 'NONE',  ( -59.83472345504510770, -87.44614099429800547, 21.65063509461101532 ) ) ;
#7029 = AXIS2_PLACEMENT_3D ( 'NONE', #4138, #4339, #14481 ) ;
#7030 = VECTOR ( 'NONE', #449, 1000.000000000000000 ) ;
#7031 = EDGE_CURVE ( 'NONE', #9513, #12208, #14074, .T. ) ;
#7032 = CARTESIAN_POINT ( 'NONE',  ( -94.14047854185179176, 6.938893903907228378E-15, 35.00000000000000000 ) ) ;
#7033 = EDGE_LOOP ( 'NONE', ( #6045, #7245 ) ) ;
#7034 = CARTESIAN_POINT ( 'NONE',  ( -24.27922930231443743, -81.80638607452326028, 1.424741226644455312E-14 ) ) ;
#7035 = DIRECTION ( 'NONE',  ( -0.1566598588826321747, 0.9876526153536343555, 0.000000000000000000 ) ) ;
#7036 = LINE ( 'NONE', #1340, #11176 ) ;
#7037 = AXIS2_PLACEMENT_3D ( 'NONE', #15615, #9670, #12398 ) ;
#7038 = CARTESIAN_POINT ( 'NONE',  ( -54.44226908077801141, -28.88533033409540351, 8.660254037844417496 ) ) ;
#7039 = CARTESIAN_POINT ( 'NONE',  ( -76.66445292623467367, -32.41017715895461038, -12.99038105676658006 ) ) ;
#7040 = FACE_OUTER_BOUND ( 'NONE', #2708, .T. ) ;
#7041 = DIRECTION ( 'NONE',  ( -1.000000000000000000, 0.000000000000000000, 0.000000000000000000 ) ) ;
#7042 = AXIS2_PLACEMENT_3D ( 'NONE', #14871, #11723, #17836 ) ;
#7043 = DIRECTION ( 'NONE',  ( -0.9826218788918641422, -0.1856185419698762606, 0.000000000000000000 ) ) ;
#7044 = LINE ( 'NONE', #12789, #10792 ) ;
#7045 = ORIENTED_EDGE ( 'NONE', *, *, #14267, .T. ) ;
#7046 = TOROIDAL_SURFACE ( 'NONE', #3357, 12.83663829214476060, 3.000000000000000000 ) ;
#7047 = DIRECTION ( 'NONE',  ( -0.000000000000000000, -0.000000000000000000, -1.000000000000000000 ) ) ;
#7048 = FACE_OUTER_BOUND ( 'NONE', #17667, .T. ) ;
#7049 = ORIENTED_EDGE ( 'NONE', *, *, #5461, .T. ) ;
#7050 = ORIENTED_EDGE ( 'NONE', *, *, #16699, .F. ) ;
#7051 = CARTESIAN_POINT ( 'NONE',  ( -53.74408945216072198, -23.71207746900332225, -8.660254037844380193 ) ) ;
#7052 = FACE_BOUND ( 'NONE', #3040, .T. ) ;
#7053 = VECTOR ( 'NONE', #6829, 1000.000000000000000 ) ;
#7054 = EDGE_CURVE ( 'NONE', #10692, #17807, #2709, .T. ) ;
#7055 = DIRECTION ( 'NONE',  ( 0.000000000000000000, 0.000000000000000000, 1.000000000000000000 ) ) ;
#7056 = ORIENTED_EDGE ( 'NONE', *, *, #8959, .F. ) ;
#7057 = STYLED_ITEM ( 'NONE', ( #3210 ), #2480 ) ;
#7058 = CARTESIAN_POINT ( 'NONE',  ( -31.52190560670403841, -20.18723064414410828, -12.99038105676658006 ) ) ;
#7059 = EDGE_CURVE ( 'NONE', #9193, #9534, #332, .T. ) ;
#7060 = ORIENTED_EDGE ( 'NONE', *, *, #13715, .F. ) ;
#7061 = AXIS2_PLACEMENT_3D ( 'NONE', #2008, #13551, #4931 ) ;
#7062 = DIRECTION ( 'NONE',  ( -0.9876526153536341335, -0.1566598588826327021, 0.000000000000000000 ) ) ;
#7063 = DIRECTION ( 'NONE',  ( 0.000000000000000000, 0.000000000000000000, 1.000000000000000000 ) ) ;
#7064 = DIRECTION ( 'NONE',  ( -0.1566598588826321192, 0.9876526153536342445, 7.798540720466730171E-17 ) ) ;
#7065 = DIRECTION ( 'NONE',  ( 0.000000000000000000, 0.000000000000000000, 1.000000000000000000 ) ) ;
#7066 = FACE_BOUND ( 'NONE', #18470, .T. ) ;
#7067 = DIRECTION ( 'NONE',  ( -0.9876526153536341335, -0.1566598588826327021, 0.000000000000000000 ) ) ;
#7068 = ORIENTED_EDGE ( 'NONE', *, *, #6669, .T. ) ;
#7069 = ORIENTED_EDGE ( 'NONE', *, *, #13853, .F. ) ;
#7070 = ORIENTED_EDGE ( 'NONE', *, *, #1933, .F. ) ;
#7071 = ORIENTED_EDGE ( 'NONE', *, *, #18192, .F. ) ;
#7072 = CARTESIAN_POINT ( 'NONE',  ( 55.85952145814821534, 6.938893903907228378E-15, -24.99999999999999289 ) ) ;
#7073 = EDGE_LOOP ( 'NONE', ( #12749, #10474, #470, #9876 ) ) ;
#7074 = ORIENTED_EDGE ( 'NONE', *, *, #2995, .T. ) ;
#7075 = LINE ( 'NONE', #9881, #10929 ) ;
#7076 = CARTESIAN_POINT ( 'NONE',  ( 3.868870235264020963, -77.34158009636824715, 1.077796531449093893E-14 ) ) ;
#7077 = VECTOR ( 'NONE', #17840, 1000.000000000000227 ) ;
#7078 = EDGE_CURVE ( 'NONE', #9210, #17772, #17313, .T. ) ;
#7079 = CYLINDRICAL_SURFACE ( 'NONE', #10574, 1.500000000000001554 ) ;
#7080 = CARTESIAN_POINT ( 'NONE',  ( -75.96627329761737712, -27.23692429386253977, 4.330127018922218518 ) ) ;
#7081 = EDGE_CURVE ( 'NONE', #17878, #14934, #18540, .T. ) ;
#7082 = DIRECTION ( 'NONE',  ( -0.1566598588826321192, 0.9876526153536342445, 7.798540720466730171E-17 ) ) ;
#7083 = DIRECTION ( 'NONE',  ( -0.1566598588826321192, 0.9876526153536342445, 7.798540720466730171E-17 ) ) ;
#7084 = DIRECTION ( 'NONE',  ( -0.1566598588826321192, 0.9876526153536342445, 7.798540720466730171E-17 ) ) ;
#7085 = DIRECTION ( 'NONE',  ( 0.000000000000000000, 0.000000000000000000, 1.000000000000000000 ) ) ;
#7086 = ORIENTED_EDGE ( 'NONE', *, *, #4861, .F. ) ;
#7087 = ORIENTED_EDGE ( 'NONE', *, *, #1244, .T. ) ;
#7088 = CIRCLE ( 'NONE', #4326, 1.500000000000000888 ) ;
#7089 = LINE ( 'NONE', #12461, #5160 ) ;
#7090 = DIRECTION ( 'NONE',  ( 0.000000000000000000, 1.000000000000000000, 1.991237296706374949E-16 ) ) ;
#7091 = CARTESIAN_POINT ( 'NONE',  ( -58.84707083969148300, -87.28948113541537168, 1.424741226644455312E-14 ) ) ;
#7092 = VERTEX_POINT ( 'NONE', #13883 ) ;
#7093 = EDGE_CURVE ( 'NONE', #10493, #202, #9637, .T. ) ;
#7094 = ORIENTED_EDGE ( 'NONE', *, *, #13085, .T. ) ;
#7095 = CYLINDRICAL_SURFACE ( 'NONE', #13939, 1.500000000000001554 ) ;
#7096 = ADVANCED_FACE ( 'NONE', ( #18398 ), #5468, .F. ) ;
#7097 = DIRECTION ( 'NONE',  ( -0.1566598588826321192, 0.9876526153536342445, 7.798540720466730171E-17 ) ) ;
#7098 = EDGE_CURVE ( 'NONE', #272, #2139, #8812, .T. ) ;
#7099 = EDGE_CURVE ( 'NONE', #6259, #13724, #2136, .T. ) ;
#7100 = DIRECTION ( 'NONE',  ( -0.1566598588826321747, 0.9876526153536343555, 0.000000000000000000 ) ) ;
#7101 = ADVANCED_FACE ( 'NONE', ( #1218 ), #11226, .T. ) ;
#7102 = DIRECTION ( 'NONE',  ( -0.9876526153536336894, -0.1566598588826349503, 0.000000000000000000 ) ) ;
#7103 = SURFACE_STYLE_FILL_AREA ( #1317 ) ;
#7104 = EDGE_CURVE ( 'NONE', #15556, #6894, #13026, .T. ) ;
#7105 = EDGE_LOOP ( 'NONE', ( #2415, #1410, #10152, #326, #12219 ) ) ;
#7106 = DIRECTION ( 'NONE',  ( 0.000000000000000000, 0.000000000000000000, 1.000000000000000000 ) ) ;
#7107 = VERTEX_POINT ( 'NONE', #8679 ) ;
#7108 = CYLINDRICAL_SURFACE ( 'NONE', #5952, 1.500000000000001554 ) ;
#7109 = CARTESIAN_POINT ( 'NONE',  ( -67.73594437787414790, -88.69941986535906153, -12.99038105676658539 ) ) ;
#7110 = EDGE_LOOP ( 'NONE', ( #14339, #6451, #5368, #7679 ) ) ;
#7111 = FACE_OUTER_BOUND ( 'NONE', #12997, .T. ) ;
#7112 = DIRECTION ( 'NONE',  ( -0.1566598588826321192, 0.9876526153536342445, 7.798540720466731404E-17 ) ) ;
#7114 = EDGE_LOOP ( 'NONE', ( #4335, #16149 ) ) ;
#7113 = CARTESIAN_POINT ( 'NONE',  ( -72.01566283620284992, -26.61028485833202240, 17.32050807568881723 ) ) ;
#7115 = ORIENTED_EDGE ( 'NONE', *, *, #11659, .F. ) ;
#7116 = ORIENTED_EDGE ( 'NONE', *, *, #1372, .F. ) ;
#7117 = CARTESIAN_POINT ( 'NONE',  ( 1.893565004556770903, -77.65489981413351472, -17.32050807568878525 ) ) ;
#7118 = EDGE_CURVE ( 'NONE', #17282, #10247, #63, .T. ) ;
#7119 = CARTESIAN_POINT ( 'NONE',  ( 0.000000000000000000, 0.000000000000000000, 35.00000000000000000 ) ) ;
#7120 = CARTESIAN_POINT ( 'NONE',  ( 73.09088021254186174, 1.387778780781445676E-14, 25.00000000000000000 ) ) ;
#7121 = CYLINDRICAL_SURFACE ( 'NONE', #10925, 1.500000000000001554 ) ;
#7122 = CARTESIAN_POINT ( 'NONE',  ( -89.99999999999998579, -35.00000000000001421, 35.00000000000000000 ) ) ;
#7123 = CARTESIAN_POINT ( 'NONE',  ( -66.29410046502154330, -30.76524864068697696, -17.32050807568878170 ) ) ;
#7124 = DIRECTION ( 'NONE',  ( 1.000000000000000000, 0.000000000000000000, -0.000000000000000000 ) ) ;
#7125 = FACE_BOUND ( 'NONE', #6872, .T. ) ;
#7126 = ADVANCED_FACE ( 'NONE', ( #16073 ), #7095, .F. ) ;
#7127 = CIRCLE ( 'NONE', #3153, 1.500000000000000888 ) ;
#7128 = ORIENTED_EDGE ( 'NONE', *, *, #17030, .F. ) ;
#7129 = EDGE_LOOP ( 'NONE', ( #8561, #9311, #18308, #5433 ) ) ;
#7130 = FACE_OUTER_BOUND ( 'NONE', #12820, .T. ) ;
#7131 = ORIENTED_EDGE ( 'NONE', *, *, #11680, .F. ) ;
#7132 = ORIENTED_EDGE ( 'NONE', *, *, #8627, .T. ) ;
#7133 = CARTESIAN_POINT ( 'NONE',  ( -51.43967622453926936, -86.11453219379563961, 4.330127018922213189 ) ) ;
#7134 = VERTEX_POINT ( 'NONE', #3076 ) ;
#7135 = CARTESIAN_POINT ( 'NONE',  ( 10.28861223506262412, -76.32329101363113466, 17.32050807568880657 ) ) ;
#7136 = FACE_BOUND ( 'NONE', #17729, .T. ) ;
#7137 = DIRECTION ( 'NONE',  ( 0.000000000000000000, 0.000000000000000000, 1.000000000000000000 ) ) ;
#7138 = AXIS2_PLACEMENT_3D ( 'NONE', #17124, #18486, #16753 ) ;
#7139 = ORIENTED_EDGE ( 'NONE', *, *, #890, .T. ) ;
#7140 = DIRECTION ( 'NONE',  ( -0.9876526153536336894, -0.1566598588826349503, 0.000000000000000000 ) ) ;
#7141 = FACE_BOUND ( 'NONE', #9438, .T. ) ;
#7142 = EDGE_CURVE ( 'NONE', #4359, #7782, #11215, .T. ) ;
#7143 = ORIENTED_EDGE ( 'NONE', *, *, #18681, .T. ) ;
#7144 = DIRECTION ( 'NONE',  ( -0.1566598588826321192, 0.9876526153536342445, 7.798540720466731404E-17 ) ) ;
#7145 = DIRECTION ( 'NONE',  ( -0.9876526153536336894, -0.1566598588826349503, 0.000000000000000000 ) ) ;
#7146 = CARTESIAN_POINT ( 'NONE',  ( 0.000000000000000000, 0.000000000000000000, -35.00000000000000000 ) ) ;
#7147 = EDGE_LOOP ( 'NONE', ( #1967, #10211 ) ) ;
#7148 = CARTESIAN_POINT ( 'NONE',  ( 0.5768043922889515285, -15.09578523045857601, -8.660254037844383745 ) ) ;
#7149 = EDGE_CURVE ( 'NONE', #6686, #18200, #10898, .T. ) ;
#7150 = VECTOR ( 'NONE', #11090, 1000.000000000000000 ) ;
#7151 = ORIENTED_EDGE ( 'NONE', *, *, #10376, .T. ) ;
#7152 = ORIENTED_EDGE ( 'NONE', *, *, #17460, .T. ) ;
#7153 = ORIENTED_EDGE ( 'NONE', *, *, #1649, .F. ) ;
#7154 = DIRECTION ( 'NONE',  ( -0.1566598588826321192, 0.9876526153536342445, 7.798540720466731404E-17 ) ) ;
#7155 = ORIENTED_EDGE ( 'NONE', *, *, #1735, .F. ) ;
#7156 = VERTEX_POINT ( 'NONE', #11596 ) ;
#7157 = FACE_BOUND ( 'NONE', #15765, .T. ) ;
#7158 = DIRECTION ( 'NONE',  ( -0.1566598588826321192, 0.9876526153536342445, 7.798540720466730171E-17 ) ) ;
#7159 = CIRCLE ( 'NONE', #7452, 1.500000000000000888 ) ;
#7160 = CARTESIAN_POINT ( 'NONE',  ( -0.5755665338273089349, -78.04654946134009208, -4.330127018922185655 ) ) ;
#7161 = CARTESIAN_POINT ( 'NONE',  ( -10.78120068427780964, -16.89737360760884144, 17.32050807568881012 ) ) ;
#7162 = DIRECTION ( 'NONE',  ( -0.1566598588826321192, 0.9876526153536342445, 7.798540720466731404E-17 ) ) ;
#7163 = DIRECTION ( 'NONE',  ( -0.1566598588826321192, 0.9876526153536342445, 7.798540720466730171E-17 ) ) ;
#7164 = ORIENTED_EDGE ( 'NONE', *, *, #22, .F. ) ;
#7165 = CARTESIAN_POINT ( 'NONE',  ( -173.9176162982875269, 56.15916356109917729, 3.150553392547033482 ) ) ;
#7166 = CARTESIAN_POINT ( 'NONE',  ( -70.24471092643608472, -31.39188807621751209, 4.330127018922217630 ) ) ;
#7167 = CARTESIAN_POINT ( 'NONE',  ( 0.000000000000000000, 0.000000000000000000, 25.00000000000000000 ) ) ;
#7168 = CYLINDRICAL_SURFACE ( 'NONE', #6530, 1.500000000000001554 ) ;
#7169 = EDGE_LOOP ( 'NONE', ( #9140, #366 ) ) ;
#7170 = ORIENTED_EDGE ( 'NONE', *, *, #148, .T. ) ;
#7171 = DIRECTION ( 'NONE',  ( -0.9876526153536336894, -0.1566598588826349503, 0.000000000000000000 ) ) ;
#7172 = CIRCLE ( 'NONE', #6869, 1.500000000000000000 ) ;
#7173 = ADVANCED_FACE ( 'NONE', ( #17507 ), #1311, .T. ) ;
#7174 = DIRECTION ( 'NONE',  ( -0.9876526153536336894, -0.1566598588826349503, 0.000000000000000000 ) ) ;
#7175 = DIRECTION ( 'NONE',  ( 1.000000000000000000, 0.000000000000000000, 0.000000000000000000 ) ) ;
#7176 = AXIS2_PLACEMENT_3D ( 'NONE', #9911, #8609, #15695 ) ;
#7177 = ORIENTED_EDGE ( 'NONE', *, *, #15412, .T. ) ;
#7178 = CARTESIAN_POINT ( 'NONE',  ( -63.78533391645962780, -88.07278042982852639, 1.424741226644455312E-14 ) ) ;
#7179 = EDGE_CURVE ( 'NONE', #13174, #9184, #6703, .T. ) ;
#7180 = ORIENTED_EDGE ( 'NONE', *, *, #10884, .F. ) ;
#7181 = DIRECTION ( 'NONE',  ( -0.9876526153536341335, -0.1566598588826327021, 0.000000000000000000 ) ) ;
#7182 = DIRECTION ( 'NONE',  ( -0.1566598588826321192, 0.9876526153536342445, 7.798540720466731404E-17 ) ) ;
#7183 = AXIS2_PLACEMENT_3D ( 'NONE', #186, #14775, #16406 ) ;
#7184 = DIRECTION ( 'NONE',  ( -0.1566598588826321192, 0.9876526153536342445, 7.798540720466731404E-17 ) ) ;
#7185 = DIRECTION ( 'NONE',  ( -0.1566598588826321192, 0.9876526153536342445, 7.798540720466731404E-17 ) ) ;
#7186 = VERTEX_POINT ( 'NONE', #7444 ) ;
#7187 = CYLINDRICAL_SURFACE ( 'NONE', #589, 1.500000000000001554 ) ;
#7188 = AXIS2_PLACEMENT_3D ( 'NONE', #7454, #4876, #16366 ) ;
#7189 = EDGE_CURVE ( 'NONE', #9493, #16874, #9107, .T. ) ;
#7190 = DIRECTION ( 'NONE',  ( 0.000000000000000000, 0.000000000000000000, 1.000000000000000000 ) ) ;
#7191 = AXIS2_PLACEMENT_3D ( 'NONE', #10403, #11987, #382 ) ;
#7192 = FACE_OUTER_BOUND ( 'NONE', #36, .T. ) ;
#7193 = CARTESIAN_POINT ( 'NONE',  ( -28.06512145296634486, -19.63892113805489359, -21.65063509461098334 ) ) ;
#7194 = EDGE_LOOP ( 'NONE', ( #10891, #17833, #2504, #2736 ) ) ;
#7195 = VERTEX_POINT ( 'NONE', #11406 ) ;
#7196 = CARTESIAN_POINT ( 'NONE',  ( -39.62747985047355570, -26.53543245085592517, 1.175313729581431390E-14 ) ) ;
#7197 = VECTOR ( 'NONE', #16186, 1000.000000000000000 ) ;
#7199 = EDGE_LOOP ( 'NONE', ( #1626, #6356, #805, #4962 ) ) ;
#7198 = DIRECTION ( 'NONE',  ( -0.9876526153536336894, -0.1566598588826349503, 0.000000000000000000 ) ) ;
#7200 = ORIENTED_EDGE ( 'NONE', *, *, #10771, .F. ) ;
#7201 = CIRCLE ( 'NONE', #8976, 2.199999999999993516 ) ;
#7202 = EDGE_CURVE ( 'NONE', #3195, #13266, #11507, .T. ) ;
#7203 = ADVANCED_FACE ( 'NONE', ( #11770 ), #5928, .F. ) ;
#7204 = ORIENTED_EDGE ( 'NONE', *, *, #9408, .F. ) ;
#7205 = EDGE_LOOP ( 'NONE', ( #10066, #2824, #5606, #3944 ) ) ;
#7206 = EDGE_CURVE ( 'NONE', #9188, #15855, #2456, .T. ) ;
#7207 = AXIS2_PLACEMENT_3D ( 'NONE', #4005, #9808, #1300 ) ;
#7208 = AXIS2_PLACEMENT_3D ( 'NONE', #18291, #2410, #3624 ) ;
#7209 = DIRECTION ( 'NONE',  ( -0.9876526153536336894, -0.1566598588826349503, 0.000000000000000000 ) ) ;
#7210 = AXIS2_PLACEMENT_3D ( 'NONE', #10363, #3429, #4768 ) ;
#7211 = FACE_OUTER_BOUND ( 'NONE', #16378, .T. ) ;
#7212 = DIRECTION ( 'NONE',  ( -0.1566598588826321192, 0.9876526153536342445, 7.798540720466730171E-17 ) ) ;
#7213 = EDGE_LOOP ( 'NONE', ( #6467, #15 ) ) ;
#7214 = DIRECTION ( 'NONE',  ( -0.1566598588826321192, 0.9876526153536342445, 7.798540720466730171E-17 ) ) ;
#7215 = CARTESIAN_POINT ( 'NONE',  ( -5.513829610595458064, -78.82984875575326100, 4.330127018922213189 ) ) ;
#7216 = CARTESIAN_POINT ( 'NONE',  ( -9.504075082187823043, -21.75730675493566579, 12.99038105676661381 ) ) ;
#7217 = CARTESIAN_POINT ( 'NONE',  ( 4.362696542940843081, -77.26325016692693737, -21.65063509461098690 ) ) ;
#7218 = CARTESIAN_POINT ( 'NONE',  ( -70.24471092643608472, -31.39188807621751209, -12.99038105676658006 ) ) ;
#7219 = FACE_OUTER_BOUND ( 'NONE', #8816, .T. ) ;
#7220 = CARTESIAN_POINT ( 'NONE',  ( -4.361458684479201153, -15.87908452487173427, -8.660254037844383745 ) ) ;
#7222 = ORIENTED_EDGE ( 'NONE', *, *, #6505, .T. ) ;
#7221 = DIRECTION ( 'NONE',  ( -0.1566598588826321192, 0.9876526153536342445, 7.798540720466730171E-17 ) ) ;
#7224 = ORIENTED_EDGE ( 'NONE', *, *, #3378, .F. ) ;
#7223 = EDGE_CURVE ( 'NONE', #15023, #2144, #4216, .T. ) ;
#7225 = LINE ( 'NONE', #12971, #275 ) ;
#7226 = ORIENTED_EDGE ( 'NONE', *, *, #15478, .T. ) ;
#7227 = ORIENTED_EDGE ( 'NONE', *, *, #1018, .F. ) ;
#7228 = CARTESIAN_POINT ( 'NONE',  ( -52.75643683680709728, -23.55541761012068491, -21.65063509461098334 ) ) ;
#7229 = AXIS2_PLACEMENT_3D ( 'NONE', #10682, #15042, #6447 ) ;
#7230 = CARTESIAN_POINT ( 'NONE',  ( -7.982961148979534016, -79.22149840295983836, 17.32050807568880657 ) ) ;
#7231 = AXIS2_PLACEMENT_3D ( 'NONE', #12401, #12106, #4822 ) ;
#7232 = CARTESIAN_POINT ( 'NONE',  ( -77.11857033228203306, -1.071618245585014506, -6.007947165629304642 ) ) ;
#7233 = AXIS2_PLACEMENT_3D ( 'NONE', #7872, #11911, #3486 ) ;
#7234 = DIRECTION ( 'NONE',  ( -0.1566598588826321192, 0.9876526153536342445, 7.798540720466731404E-17 ) ) ;
#7235 = FACE_BOUND ( 'NONE', #16449, .T. ) ;
#7236 = EDGE_LOOP ( 'NONE', ( #1678, #9793 ) ) ;
#7237 = DIRECTION ( 'NONE',  ( -0.1566598588826321747, 0.9876526153536343555, 0.000000000000000000 ) ) ;
#7238 = CARTESIAN_POINT ( 'NONE',  ( -47.48906576312474215, -85.48789275826510448, -8.660254037844385522 ) ) ;
#7239 = AXIS2_PLACEMENT_3D ( 'NONE', #3959, #9934, #14315 ) ;
#7240 = DIRECTION ( 'NONE',  ( -1.000000000000000000, 0.000000000000000000, 0.000000000000000000 ) ) ;
#7241 = AXIS2_PLACEMENT_3D ( 'NONE', #16622, #17696, #4664 ) ;
#7242 = ORIENTED_EDGE ( 'NONE', *, *, #1522, .T. ) ;
#7243 =( GEOMETRIC_REPRESENTATION_CONTEXT ( 3 ) GLOBAL_UNCERTAINTY_ASSIGNED_CONTEXT ( ( #6080 ) ) GLOBAL_UNIT_ASSIGNED_CONTEXT ( ( #10952, #3739, #15319 ) ) REPRESENTATION_CONTEXT ( 'NONE', 'WORKASPACE' ) );
#7244 = ORIENTED_EDGE ( 'NONE', *, *, #4293, .T. ) ;
#7245 = ORIENTED_EDGE ( 'NONE', *, *, #1244, .F. ) ;
#7246 = CYLINDRICAL_SURFACE ( 'NONE', #3063, 1.500000000000001554 ) ;
#7247 = VERTEX_POINT ( 'NONE', #9997 ) ;
#7248 = LINE ( 'NONE', #11743, #4581 ) ;
#7249 = EDGE_CURVE ( 'NONE', #8900, #17816, #15154, .T. ) ;
#7250 = AXIS2_PLACEMENT_3D ( 'NONE', #4174, #7234, #12982 ) ;
#7251 = LINE ( 'NONE', #43, #3595 ) ;
#7252 = ADVANCED_FACE ( 'NONE', ( #5849 ), #17334, .F. ) ;
#7253 = ORIENTED_EDGE ( 'NONE', *, *, #10015, .T. ) ;
#7254 = CIRCLE ( 'NONE', #12661, 2.200000000000000178 ) ;
#7255 = EDGE_CURVE ( 'NONE', #12715, #14620, #2880, .T. ) ;
#7256 = VECTOR ( 'NONE', #17657, 1000.000000000000000 ) ;
#7257 = DIRECTION ( 'NONE',  ( -0.000000000000000000, -0.000000000000000000, -1.000000000000000000 ) ) ;
#7258 = LINE ( 'NONE', #8855, #18265 ) ;
#7259 = SHAPE_DEFINITION_REPRESENTATION ( #16674, #17876 ) ;
#7260 = DIRECTION ( 'NONE',  ( -0.9876526153536344665, -0.1566598588826304539, 0.000000000000000000 ) ) ;
#7261 = DIRECTION ( 'NONE',  ( 3.208277787129350839E-17, 0.000000000000000000, -1.000000000000000000 ) ) ;
#7262 = VECTOR ( 'NONE', #1291, 1000.000000000000000 ) ;
#7263 = CARTESIAN_POINT ( 'NONE',  ( -70.61186533023291645, 45.26035146208064219, -4.992628012786330949 ) ) ;
#7264 = CYLINDRICAL_SURFACE ( 'NONE', #5372, 1.500000000000001554 ) ;
#7265 = ORIENTED_EDGE ( 'NONE', *, *, #5588, .T. ) ;
#7266 = ORIENTED_EDGE ( 'NONE', *, *, #10730, .F. ) ;
#7267 = CARTESIAN_POINT ( 'NONE',  ( 0.000000000000000000, 0.000000000000000000, 30.00000000000000000 ) ) ;
#7268 = AXIS2_PLACEMENT_3D ( 'NONE', #3285, #14772, #11628 ) ;
#7269 = CARTESIAN_POINT ( 'NONE',  ( -6.007655918272284623, -78.90817868519457079, 17.32050807568880657 ) ) ;
#7270 = DIRECTION ( 'NONE',  ( -0.1566598588826321192, 0.9876526153536342445, 7.798540720466731404E-17 ) ) ;
#7271 = AXIS2_PLACEMENT_3D ( 'NONE', #17822, #16675, #12270 ) ;
#7272 = CIRCLE ( 'NONE', #17872, 1.500000000000000444 ) ;
#7273 = AXIS2_PLACEMENT_3D ( 'NONE', #1280, #5822, #13092 ) ;
#7274 = ORIENTED_EDGE ( 'NONE', *, *, #11042, .F. ) ;
#7275 = CARTESIAN_POINT ( 'NONE',  ( -127.1404785156000941, -15.31509901360653636, 2.500000000000000000 ) ) ;
#7276 = DIRECTION ( 'NONE',  ( 1.000000000000000000, 0.000000000000000000, 0.000000000000000000 ) ) ;
#7277 = EDGE_CURVE ( 'NONE', #13253, #3382, #13507, .T. ) ;
#7278 = CIRCLE ( 'NONE', #17891, 1.500000000000000444 ) ;
#7279 = CARTESIAN_POINT ( 'NONE',  ( 0.000000000000000000, 0.000000000000000000, -25.00000000000000000 ) ) ;
#7280 = DIRECTION ( 'NONE',  ( -1.000000000000000000, 0.000000000000000000, 0.000000000000000000 ) ) ;
#7281 = PRODUCT_CONTEXT ( 'NONE', #9191, 'mechanical' ) ;
#7282 = VERTEX_POINT ( 'NONE', #14459 ) ;
#7283 = AXIS2_PLACEMENT_3D ( 'NONE', #9729, #9522, #17036 ) ;
#7284 = FACE_OUTER_BOUND ( 'NONE', #7995, .T. ) ;
#7285 = VECTOR ( 'NONE', #1212, 1000.000000000000000 ) ;
#7286 = EDGE_LOOP ( 'NONE', ( #16445, #12100 ) ) ;
#7287 = CYLINDRICAL_SURFACE ( 'NONE', #11961, 1.500000000000001554 ) ;
#7288 = EDGE_CURVE ( 'NONE', #13047, #15200, #4864, .T. ) ;
#7289 = CARTESIAN_POINT ( 'NONE',  ( -81.37336115545215875, 3.066817964230565963, 2.499999999999999556 ) ) ;
#7290 = ORIENTED_EDGE ( 'NONE', *, *, #316, .T. ) ;
#7291 = ORIENTED_EDGE ( 'NONE', *, *, #8427, .F. ) ;
#7292 = CYLINDRICAL_SURFACE ( 'NONE', #14264, 2.000000000000000000 ) ;
#7293 = EDGE_CURVE ( 'NONE', #14073, #56, #15468, .T. ) ;
#7294 = VERTEX_POINT ( 'NONE', #10458 ) ;
#7295 = CARTESIAN_POINT ( 'NONE',  ( -53.74408945216069355, -23.71207746900333291, 17.32050807568882078 ) ) ;
#7296 = CIRCLE ( 'NONE', #4548, 144.0000000000000284 ) ;
#7297 = ORIENTED_EDGE ( 'NONE', *, *, #5125, .T. ) ;
#7298 = ORIENTED_EDGE ( 'NONE', *, *, #8750, .T. ) ;
#7299 = ORIENTED_EDGE ( 'NONE', *, *, #6366, .T. ) ;
#7300 = CIRCLE ( 'NONE', #15457, 1.500000000000000444 ) ;
#7301 = DIRECTION ( 'NONE',  ( -0.9876526153536341335, -0.1566598588826327021, 0.000000000000000000 ) ) ;
#7302 = DIRECTION ( 'NONE',  ( -0.9876526153536341335, -0.1566598588826327021, 0.000000000000000000 ) ) ;
#7303 = EDGE_CURVE ( 'NONE', #8040, #11020, #16687, .T. ) ;
#7304 = CARTESIAN_POINT ( 'NONE',  ( -70.04035760549561473, -26.29696514056675127, 8.660254037844417496 ) ) ;
#7305 = DIRECTION ( 'NONE',  ( -0.9876526153536341335, -0.1566598588826327021, 0.000000000000000000 ) ) ;
#7306 = CARTESIAN_POINT ( 'NONE',  ( 3.231158466157545206, -19.73726462726228092, 35.00000000000000000 ) ) ;
#7307 = AXIS2_PLACEMENT_3D ( 'NONE', #808, #6694, #13676 ) ;
#7308 = EDGE_CURVE ( 'NONE', #17245, #15425, #7724, .T. ) ;
#7309 = CARTESIAN_POINT ( 'NONE',  ( -24.11451099155181055, -19.01228170252437266, -17.32050807568878170 ) ) ;
#7310 = ORIENTED_EDGE ( 'NONE', *, *, #8193, .T. ) ;
#7311 = DIRECTION ( 'NONE',  ( 0.000000000000000000, 0.000000000000000000, 1.000000000000000000 ) ) ;
#7312 = EDGE_CURVE ( 'NONE', #3161, #4161, #17622, .T. ) ;
#7313 = CARTESIAN_POINT ( 'NONE',  ( -17.40529600501688279, -23.01058562599671831, 4.330127018922217630 ) ) ;
#7314 = FACE_OUTER_BOUND ( 'NONE', #14316, .T. ) ;
#7316 = ORIENTED_EDGE ( 'NONE', *, *, #16792, .T. ) ;
#7315 = CARTESIAN_POINT ( 'NONE',  ( -45.55339554259532520, -27.47539160415171722, 12.99038105676661736 ) ) ;
#7317 = AXIS2_PLACEMENT_3D ( 'NONE', #7367, #15794, #5759 ) ;
#7318 = ORIENTED_EDGE ( 'NONE', *, *, #17546, .T. ) ;
#7319 = CARTESIAN_POINT ( 'NONE',  ( -90.00000000000001421, 34.99999999999996447, 2.500000000000000000 ) ) ;
#7320 = DIRECTION ( 'NONE',  ( -0.1566598588826321192, 0.9876526153536342445, 7.798540720466730171E-17 ) ) ;
#7321 = EDGE_LOOP ( 'NONE', ( #3043, #8917, #11629, #15748 ) ) ;
#7322 = ORIENTED_EDGE ( 'NONE', *, *, #2633, .F. ) ;
#7323 = ORIENTED_EDGE ( 'NONE', *, *, #8041, .T. ) ;
#7324 = DIRECTION ( 'NONE',  ( -0.1566598588826321192, 0.9876526153536342445, 7.798540720466730171E-17 ) ) ;
#7325 = DIRECTION ( 'NONE',  ( -0.1566598588826321192, 0.9876526153536342445, 7.798540720466730171E-17 ) ) ;
#7326 = ORIENTED_EDGE ( 'NONE', *, *, #11096, .F. ) ;
#7327 = AXIS2_PLACEMENT_3D ( 'NONE', #16830, #8370, #10813 ) ;
#7328 = CARTESIAN_POINT ( 'NONE',  ( -51.27495791377661760, -23.32042782179675555, 21.65063509461102242 ) ) ;
#7329 = ADVANCED_FACE ( 'NONE', ( #1846 ), #12152, .F. ) ;
#7330 = CIRCLE ( 'NONE', #13348, 1.499999999999999556 ) ;
#7331 = EDGE_CURVE ( 'NONE', #14760, #13568, #15167, .T. ) ;
#7332 = EDGE_CURVE ( 'NONE', #6192, #7092, #7814, .T. ) ;
#7333 = LINE ( 'NONE', #9380, #313 ) ;
#7334 = CARTESIAN_POINT ( 'NONE',  ( -21.81009776393036503, -81.41473642731666871, -21.65063509461098690 ) ) ;
#7335 = ORIENTED_EDGE ( 'NONE', *, *, #7613, .F. ) ;
#7336 = ORIENTED_EDGE ( 'NONE', *, *, #4626, .F. ) ;
#7337 = CIRCLE ( 'NONE', #14439, 1.500000000000000444 ) ;
#7338 = AXIS2_PLACEMENT_3D ( 'NONE', #11084, #16909, #17006 ) ;
#7339 = CARTESIAN_POINT ( 'NONE',  ( -90.00000000000000000, 34.99999999999999289, 100.5765140304660861 ) ) ;
#7340 = CARTESIAN_POINT ( 'NONE',  ( -10.98555400521827963, -21.99229654325962002, -21.65063509461098334 ) ) ;
#7341 = FACE_OUTER_BOUND ( 'NONE', #16762, .T. ) ;
#7342 = ORIENTED_EDGE ( 'NONE', *, *, #6023, .T. ) ;
#7343 = CIRCLE ( 'NONE', #11827, 1.499999999999999556 ) ;
#7344 = ORIENTED_EDGE ( 'NONE', *, *, #17175, .T. ) ;
#7345 = ORIENTED_EDGE ( 'NONE', *, *, #362, .F. ) ;
#7346 = DIRECTION ( 'NONE',  ( 0.000000000000000000, 0.000000000000000000, 1.000000000000000000 ) ) ;
#7347 = ORIENTED_EDGE ( 'NONE', *, *, #5478, .F. ) ;
#7348 = VERTEX_POINT ( 'NONE', #10653 ) ;
#7349 = CARTESIAN_POINT ( 'NONE',  ( -57.85941822433785120, -87.13282127653275211, 21.65063509461101532 ) ) ;
#7350 = EDGE_CURVE ( 'NONE', #16387, #10257, #16450, .T. ) ;
#7351 = DIRECTION ( 'NONE',  ( -0.1566598588826321192, 0.9876526153536342445, 7.798540720466730171E-17 ) ) ;
#7352 = ORIENTED_EDGE ( 'NONE', *, *, #7503, .T. ) ;
#7353 = SHAPE_REPRESENTATION ( 'BR-825', ( #13517, #8985, #837, #14750, #1742, #7208, #4154, #6295, #14454 ), #2933 ) ;
#7354 = AXIS2_PLACEMENT_3D ( 'NONE', #1226, #7011, #11319 ) ;
#7355 = CARTESIAN_POINT ( 'NONE',  ( -34.68921677370541090, -25.75213315644277046, 17.32050807568881723 ) ) ;
#7356 = FACE_OUTER_BOUND ( 'NONE', #17740, .T. ) ;
#7357 = DIRECTION ( 'NONE',  ( -0.9876526153536336894, -0.1566598588826350336, 0.000000000000000000 ) ) ;
#7358 = EDGE_CURVE ( 'NONE', #15786, #2545, #7638, .T. ) ;
#7359 = FACE_OUTER_BOUND ( 'NONE', #142, .T. ) ;
#7360 = VERTEX_POINT ( 'NONE', #13576 ) ;
#7361 = EDGE_CURVE ( 'NONE', #14719, #15217, #15481, .T. ) ;
#7362 = ORIENTED_EDGE ( 'NONE', *, *, #17537, .T. ) ;
#7363 = CARTESIAN_POINT ( 'NONE',  ( -138.4775067298212718, -42.93618108924343346, 2.500000000000000000 ) ) ;
#7364 = CARTESIAN_POINT ( 'NONE',  ( -90.00000000000000000, 34.99999999999999289, -35.00000000000000000 ) ) ;
#7365 = ORIENTED_EDGE ( 'NONE', *, *, #4087, .T. ) ;
#7366 = ORIENTED_EDGE ( 'NONE', *, *, #4321, .F. ) ;
#7367 = CARTESIAN_POINT ( 'NONE',  ( -15.92381708198642798, -22.77559583767277473, -21.65063509461098334 ) ) ;
#7368 = CARTESIAN_POINT ( 'NONE',  ( -30.73860631229088725, -25.12549372091224598, 12.99038105676661736 ) ) ;
#7369 = CARTESIAN_POINT ( 'NONE',  ( -62.13913668266656032, -25.04368626950569521, -8.660254037844380193 ) ) ;
#7370 = CARTESIAN_POINT ( 'NONE',  ( 0.5768043922889515285, -15.09578523045857601, 17.32050807568881368 ) ) ;
#7371 = AXIS2_PLACEMENT_3D ( 'NONE', #14779, #1804, #7591 ) ;
#7372 = DIRECTION ( 'NONE',  ( -0.1566598588826321747, 0.9876526153536343555, 0.000000000000000000 ) ) ;
#7373 = CARTESIAN_POINT ( 'NONE',  ( -56.21322099054479082, -24.10372711620990316, -4.330127018922180326 ) ) ;
#7374 = ADVANCED_FACE ( 'NONE', ( #6123 ), #12235, .F. ) ;
#7375 = CARTESIAN_POINT ( 'NONE',  ( -38.14600092744309734, -26.30044266253198160, -8.660254037844380193 ) ) ;
#7376 = ORIENTED_EDGE ( 'NONE', *, *, #6633, .F. ) ;
#7377 = CARTESIAN_POINT ( 'NONE',  ( -62.79768130110601021, -87.91612057094589261, -21.65063509461098690 ) ) ;
#7378 = EDGE_CURVE ( 'NONE', #4161, #1436, #17706, .T. ) ;
#7379 = EDGE_LOOP ( 'NONE', ( #879, #3050, #17474, #16226 ) ) ;
#7380 = ADVANCED_FACE ( 'NONE', ( #625 ), #13303, .F. ) ;
#7381 = CARTESIAN_POINT ( 'NONE',  ( -19.34096622554629263, -81.02308678011009135, -17.32050807568878525 ) ) ;
#7382 = ORIENTED_EDGE ( 'NONE', *, *, #8530, .T. ) ;
#7383 = ORIENTED_EDGE ( 'NONE', *, *, #15678, .T. ) ;
#7384 = CIRCLE ( 'NONE', #8886, 1.499999999999999556 ) ;
#7385 = DIRECTION ( 'NONE',  ( -0.1566598588826321192, 0.9876526153536342445, 7.798540720466730171E-17 ) ) ;
#7386 = ADVANCED_FACE ( 'NONE', ( #5039 ), #10728, .T. ) ;
#7387 = DIRECTION ( 'NONE',  ( -0.1566598588826321747, 0.9876526153536343555, 0.000000000000000000 ) ) ;
#7388 = CARTESIAN_POINT ( 'NONE',  ( -14.44233815895597672, -22.54060604934882051, -21.65063509461098334 ) ) ;
#7389 = ORIENTED_EDGE ( 'NONE', *, *, #13483, .F. ) ;
#7390 = DIRECTION ( 'NONE',  ( -0.1566598588826321747, 0.9876526153536343555, 0.000000000000000000 ) ) ;
#7391 = CARTESIAN_POINT ( 'NONE',  ( -94.14047854185177755, -35.00000000000001421, 30.00000000000002487 ) ) ;
#7392 = DIRECTION ( 'NONE',  ( -0.9876526153536341335, -0.1566598588826327021, 0.000000000000000000 ) ) ;
#7393 = CARTESIAN_POINT ( 'NONE',  ( -35.63723437888119605, -83.60797445167352748, -17.32050807568878525 ) ) ;
#7394 = EDGE_LOOP ( 'NONE', ( #13841, #2235, #5276, #10733 ) ) ;
#7395 = DIRECTION ( 'NONE',  ( 1.000000000000000000, 0.000000000000000000, 0.000000000000000000 ) ) ;
#7396 = DIRECTION ( 'NONE',  ( -1.000000000000000000, 0.000000000000000000, 0.000000000000000000 ) ) ;
#7397 = DIRECTION ( 'NONE',  ( -0.1566598588826321192, 0.9876526153536342445, 7.798540720466730171E-17 ) ) ;
#7399 = EDGE_LOOP ( 'NONE', ( #9180, #17108 ) ) ;
#7398 = LINE ( 'NONE', #1347, #5426 ) ;
#7400 = VERTEX_POINT ( 'NONE', #15101 ) ;
#7401 = DIRECTION ( 'NONE',  ( -0.1566598588826321747, 0.9876526153536343555, 0.000000000000000000 ) ) ;
#7402 = EDGE_LOOP ( 'NONE', ( #13818, #11359 ) ) ;
#7403 = EDGE_CURVE ( 'NONE', #12234, #6209, #4278, .T. ) ;
#7404 = ORIENTED_EDGE ( 'NONE', *, *, #12484, .T. ) ;
#7405 = ORIENTED_EDGE ( 'NONE', *, *, #7189, .T. ) ;
#7406 = DIRECTION ( 'NONE',  ( 0.000000000000000000, 0.000000000000000000, 1.000000000000000000 ) ) ;
#7407 = DIRECTION ( 'NONE',  ( -0.1566598588826321192, 0.9876526153536342445, 7.798540720466730171E-17 ) ) ;
#7408 = EDGE_CURVE ( 'NONE', #3070, #4072, #14272, .T. ) ;
#7409 = DIRECTION ( 'NONE',  ( 0.000000000000000000, 0.000000000000000000, 1.000000000000000000 ) ) ;
#7410 = CIRCLE ( 'NONE', #2861, 12.83663829214476060 ) ;
#7411 = CARTESIAN_POINT ( 'NONE',  ( 0.000000000000000000, 0.000000000000000000, -24.99999999999999289 ) ) ;
#7412 = ORIENTED_EDGE ( 'NONE', *, *, #5511, .T. ) ;
#7413 = EDGE_LOOP ( 'NONE', ( #1922, #4689 ) ) ;
#7414 = FACE_OUTER_BOUND ( 'NONE', #7829, .T. ) ;
#7415 = FACE_BOUND ( 'NONE', #6490, .T. ) ;
#7416 = CARTESIAN_POINT ( 'NONE',  ( 0.000000000000000000, 0.000000000000000000, -35.00000000000000000 ) ) ;
#7417 = ORIENTED_EDGE ( 'NONE', *, *, #280, .F. ) ;
#7418 = VERTEX_POINT ( 'NONE', #4771 ) ;
#7419 = ORIENTED_EDGE ( 'NONE', *, *, #13193, .F. ) ;
#7420 = CARTESIAN_POINT ( 'NONE',  ( 0.000000000000000000, 0.000000000000000000, 30.00000000000000000 ) ) ;
#7421 = EDGE_CURVE ( 'NONE', #7348, #9121, #10631, .T. ) ;
#7422 = ADVANCED_FACE ( 'NONE', ( #1194 ), #14052, .F. ) ;
#7423 = AXIS2_PLACEMENT_3D ( 'NONE', #3212, #15253, #2723 ) ;
#7424 = LINE ( 'NONE', #7349, #18263 ) ;
#7425 = EDGE_CURVE ( 'NONE', #3795, #12785, #4874, .T. ) ;
#7426 = LINE ( 'NONE', #4569, #1206 ) ;
#7427 = EDGE_LOOP ( 'NONE', ( #3337, #5795 ) ) ;
#7428 = EDGE_CURVE ( 'NONE', #3494, #1209, #7330, .T. ) ;
#7429 = VERTEX_POINT ( 'NONE', #3715 ) ;
#7430 = ADVANCED_FACE ( 'NONE', ( #2505 ), #2398, .F. ) ;
#7431 = ORIENTED_EDGE ( 'NONE', *, *, #18600, .T. ) ;
#7432 = DIRECTION ( 'NONE',  ( -0.1566598588826321192, 0.9876526153536342445, 7.798540720466731404E-17 ) ) ;
#7433 = VECTOR ( 'NONE', #16367, 1000.000000000000000 ) ;
#7434 = DIRECTION ( 'NONE',  ( 0.000000000000000000, 0.000000000000000000, 1.000000000000000000 ) ) ;
#7435 = DIRECTION ( 'NONE',  ( 1.000000000000000000, 0.000000000000000000, 0.000000000000000000 ) ) ;
#7436 = ORIENTED_EDGE ( 'NONE', *, *, #17101, .F. ) ;
#7437 = VERTEX_POINT ( 'NONE', #9607 ) ;
#7438 = LINE ( 'NONE', #1932, #18476 ) ;
#7439 = CARTESIAN_POINT ( 'NONE',  ( -39.91695283720987675, -21.51883944464649545, 21.65063509461101887 ) ) ;
#7440 = FACE_OUTER_BOUND ( 'NONE', #16231, .T. ) ;
#7441 = EDGE_CURVE ( 'NONE', #13253, #9794, #11276, .T. ) ;
#7442 = EDGE_CURVE ( 'NONE', #4836, #15547, #11005, .T. ) ;
#7443 = VERTEX_POINT ( 'NONE', #8083 ) ;
#7444 = CARTESIAN_POINT ( 'NONE',  ( -65.23030399291525327, 43.49999999999997868, 20.00000000000001776 ) ) ;
#7445 = CARTESIAN_POINT ( 'NONE',  ( -79.50650145259169221, 31.87494681980769684, 35.00000599999999906 ) ) ;
#7446 = CIRCLE ( 'NONE', #11645, 1.500000000000000888 ) ;
#7447 = EDGE_CURVE ( 'NONE', #11326, #7506, #8291, .T. ) ;
#7448 = EDGE_CURVE ( 'NONE', #10670, #14934, #1098, .T. ) ;
#7449 = DIRECTION ( 'NONE',  ( -0.9201637183752249260, -0.3915338189555018777, -3.511704013281690003E-17 ) ) ;
#7450 = DIRECTION ( 'NONE',  ( -0.1566598588826321747, 0.9876526153536343555, 0.000000000000000000 ) ) ;
#7451 = FILL_AREA_STYLE ('',( #3081 ) ) ;
#7452 = AXIS2_PLACEMENT_3D ( 'NONE', #2429, #8114, #18210 ) ;
#7453 = CARTESIAN_POINT ( 'NONE',  ( -129.1404785418517918, -2.850701963179328668, 12.74754878398196745 ) ) ;
#7454 = CARTESIAN_POINT ( 'NONE',  ( -1.892327146095121204, -15.48743487766515337, -4.330127018922183879 ) ) ;
#7455 = CARTESIAN_POINT ( 'NONE',  ( -172.7326993491721225, 43.83249341393818810, 9.951701414186830458E-16 ) ) ;
#7456 = DIRECTION ( 'NONE',  ( 0.000000000000000000, 0.000000000000000000, 1.000000000000000000 ) ) ;
#7457 = EDGE_LOOP ( 'NONE', ( #5568, #9626, #11822, #4125 ) ) ;
#7458 = ORIENTED_EDGE ( 'NONE', *, *, #14027, .T. ) ;
#7459 = DIRECTION ( 'NONE',  ( -0.1566598588826321192, 0.9876526153536342445, 7.798540720466731404E-17 ) ) ;
#7460 = VECTOR ( 'NONE', #2471, 1000.000000000000000 ) ;
#7462 = ORIENTED_EDGE ( 'NONE', *, *, #7707, .F. ) ;
#7461 = DIRECTION ( 'NONE',  ( -0.9876526153536341335, -0.1566598588826327021, 0.000000000000000000 ) ) ;
#7463 = DIRECTION ( 'NONE',  ( -0.9876526153536336894, -0.1566598588826349503, 0.000000000000000000 ) ) ;
#7464 = ORIENTED_EDGE ( 'NONE', *, *, #3146, .T. ) ;
#7465 = FACE_OUTER_BOUND ( 'NONE', #4764, .T. ) ;
#7466 = ADVANCED_FACE ( 'NONE', ( #8373 ), #8192, .F. ) ;
#7467 = LINE ( 'NONE', #4697, #10323 ) ;
#7468 = EDGE_CURVE ( 'NONE', #15912, #9201, #8825, .T. ) ;
#7469 = FACE_BOUND ( 'NONE', #13105, .T. ) ;
#7470 = CIRCLE ( 'NONE', #7176, 1.499999999999999556 ) ;
#7471 = DIRECTION ( 'NONE',  ( 0.000000000000000000, 0.000000000000000000, 1.000000000000000000 ) ) ;
#7472 = CARTESIAN_POINT ( 'NONE',  ( -64.31879523431432233, -30.45192892292171294, -17.32050807568878170 ) ) ;
#7473 = DIRECTION ( 'NONE',  ( 0.000000000000000000, 0.000000000000000000, 1.000000000000000000 ) ) ;
#7474 = EDGE_CURVE ( 'NONE', #4718, #16444, #16096, .T. ) ;
#7475 = DIRECTION ( 'NONE',  ( -0.9876526153536344665, -0.1566598588826304539, 0.000000000000000000 ) ) ;
#7476 = CYLINDRICAL_SURFACE ( 'NONE', #12881, 1.500000000000001554 ) ;
#7477 = CIRCLE ( 'NONE', #15040, 1.500000000000001332 ) ;
#7478 = CARTESIAN_POINT ( 'NONE',  ( -42.55080268635658314, -84.70459346385194976, 8.660254037844412167 ) ) ;
#7479 = DIRECTION ( 'NONE',  ( -0.1566598588826321747, 0.9876526153536343555, 0.000000000000000000 ) ) ;
#7480 = CIRCLE ( 'NONE', #18425, 1.500000000000000888 ) ;
#7482 = VERTEX_POINT ( 'NONE', #908 ) ;
#7481 = CARTESIAN_POINT ( 'NONE',  ( -40.41077914488672462, -21.59716937408779103, -17.32050807568878170 ) ) ;
#7483 = ORIENTED_EDGE ( 'NONE', *, *, #4644, .F. ) ;
#7484 = DIRECTION ( 'NONE',  ( -0.1566598588826321747, 0.9876526153536343555, 0.000000000000000000 ) ) ;
#7485 = CIRCLE ( 'NONE', #10479, 2.000000000000001776 ) ;
#7486 = EDGE_LOOP ( 'NONE', ( #1512, #8049, #13929, #15175 ) ) ;
#7487 = AXIS2_PLACEMENT_3D ( 'NONE', #4715, #16289, #9086 ) ;
#7488 = ORIENTED_EDGE ( 'NONE', *, *, #8761, .F. ) ;
#7489 = EDGE_LOOP ( 'NONE', ( #10648, #13832 ) ) ;
#7490 = CARTESIAN_POINT ( 'NONE',  ( -89.99999999999998579, -35.00000000000001421, -30.00000000000000000 ) ) ;
#7491 = DIRECTION ( 'NONE',  ( -0.1566598588826321192, 0.9876526153536342445, 7.798540720466730171E-17 ) ) ;
#7492 = AXIS2_PLACEMENT_3D ( 'NONE', #6013, #7531, #11763 ) ;
#7493 = FACE_OUTER_BOUND ( 'NONE', #2255, .T. ) ;
#7494 = EDGE_LOOP ( 'NONE', ( #15982, #16200, #11665, #17114 ) ) ;
#7495 = EDGE_CURVE ( 'NONE', #6575, #15928, #1011, .T. ) ;
#7496 = MECHANICAL_DESIGN_GEOMETRIC_PRESENTATION_REPRESENTATION (  '', ( #16262 ), #18733 ) ;
#7497 = ORIENTED_EDGE ( 'NONE', *, *, #14085, .F. ) ;
#7498 = AXIS2_PLACEMENT_3D ( 'NONE', #10455, #8945, #14823 ) ;
#7499 = CARTESIAN_POINT ( 'NONE',  ( -1.109027851681966492, -20.42569795443330349, -4.330127018922184767 ) ) ;
#7500 = APPLICATION_CONTEXT ( 'automotive_design' ) ;
#7501 = ORIENTED_EDGE ( 'NONE', *, *, #6058, .T. ) ;
#7502 = CARTESIAN_POINT ( 'NONE',  ( -42.09661138885762455, -26.92708209806250608, -4.330127018922181215 ) ) ;
#7503 = EDGE_CURVE ( 'NONE', #9998, #11443, #13003, .T. ) ;
#7504 = DIRECTION ( 'NONE',  ( -0.1566598588826321192, 0.9876526153536342445, 7.798540720466731404E-17 ) ) ;
#7505 = VERTEX_POINT ( 'NONE', #15946 ) ;
#7506 = VERTEX_POINT ( 'NONE', #2682 ) ;
#7507 = ORIENTED_EDGE ( 'NONE', *, *, #6388, .F. ) ;
#7508 = FACE_OUTER_BOUND ( 'NONE', #8338, .T. ) ;
#7509 = EDGE_LOOP ( 'NONE', ( #15898, #13828, #16248, #12132 ) ) ;
#7510 = FACE_BOUND ( 'NONE', #14641, .T. ) ;
#7511 = VECTOR ( 'NONE', #11618, 1000.000000000000000 ) ;
#7512 = DIRECTION ( 'NONE',  ( -0.1566598588826321192, 0.9876526153536342445, 7.798540720466730171E-17 ) ) ;
#7513 = ORIENTED_EDGE ( 'NONE', *, *, #6644, .T. ) ;
#7514 = FACE_OUTER_BOUND ( 'NONE', #18660, .T. ) ;
#7515 = ORIENTED_EDGE ( 'NONE', *, *, #8033, .T. ) ;
#7516 = CIRCLE ( 'NONE', #16296, 2.200000000000000622 ) ;
#7517 = DIRECTION ( 'NONE',  ( -0.9876526153536341335, -0.1566598588826327021, 0.000000000000000000 ) ) ;
#7518 = EDGE_CURVE ( 'NONE', #1621, #18301, #7248, .T. ) ;
#7519 = CIRCLE ( 'NONE', #5719, 1.500000000000000444 ) ;
#7520 = EDGE_CURVE ( 'NONE', #10837, #4610, #7075, .T. ) ;
#7521 = DIRECTION ( 'NONE',  ( -0.1566598588826321192, 0.9876526153536342445, 7.798540720466730171E-17 ) ) ;
#7522 = CIRCLE ( 'NONE', #5723, 1.500000000000001332 ) ;
#7523 = DIRECTION ( 'NONE',  ( 1.000000000000000000, -0.000000000000000000, -0.000000000000000000 ) ) ;
#7524 = PRESENTATION_LAYER_ASSIGNMENT (  '', '', ( #12022 ) ) ;
#7525 = EDGE_CURVE ( 'NONE', #9571, #14620, #7343, .T. ) ;
#7526 = CARTESIAN_POINT ( 'NONE',  ( -0.4108482230646692823, -15.25244508934120802, -12.99038105676658361 ) ) ;
#7527 = CARTESIAN_POINT ( 'NONE',  ( -53.90880776292333820, -86.50618184100221697, 8.660254037844412167 ) ) ;
#7528 = ORIENTED_EDGE ( 'NONE', *, *, #9376, .T. ) ;
#7529 = ORIENTED_EDGE ( 'NONE', *, *, #8585, .T. ) ;
#7530 = DIRECTION ( 'NONE',  ( -0.1566598588826321747, 0.9876526153536343555, 0.000000000000000000 ) ) ;
#7531 = DIRECTION ( 'NONE',  ( -0.1566598588826321192, 0.9876526153536342445, 7.798540720466731404E-17 ) ) ;
#7532 = CARTESIAN_POINT ( 'NONE',  ( -58.84707083969148300, -87.28948113541537168, -8.660254037844385522 ) ) ;
#7533 = VERTEX_POINT ( 'NONE', #2951 ) ;
#7534 = AXIS2_PLACEMENT_3D ( 'NONE', #10334, #17763, #17678 ) ;
#7535 = ORIENTED_EDGE ( 'NONE', *, *, #12086, .F. ) ;
#7536 = CARTESIAN_POINT ( 'NONE',  ( -67.73594437787414790, -88.69941986535906153, 21.65063509461101532 ) ) ;
#7537 = CIRCLE ( 'NONE', #17250, 1.500000000000001332 ) ;
#7538 = AXIS2_PLACEMENT_3D ( 'NONE', #14907, #12134, #4936 ) ;
#7539 = CARTESIAN_POINT ( 'NONE',  ( -89.99999999999998579, -35.00000000000001421, 35.00000000000000000 ) ) ;
#7540 = DIRECTION ( 'NONE',  ( -0.9539392014169452150, 0.3000000000000013212, 2.548423110585632720E-16 ) ) ;
#7541 = DIRECTION ( 'NONE',  ( 0.000000000000000000, 0.000000000000000000, 1.000000000000000000 ) ) ;
#7542 =( NAMED_UNIT ( * ) SI_UNIT ( $, .STERADIAN. ) SOLID_ANGLE_UNIT ( ) );
#7543 = ADVANCED_FACE ( 'NONE', ( #10153 ), #16110, .T. ) ;
#7544 = VECTOR ( 'NONE', #14224, 1000.000000000000227 ) ;
#7545 = ADVANCED_FACE ( 'NONE', ( #130 ), #18747, .F. ) ;
#7546 = CARTESIAN_POINT ( 'NONE',  ( -85.86167379012967160, 34.32252072304513746, 30.00000000000002487 ) ) ;
#7548 = CARTESIAN_POINT ( 'NONE',  ( -34.15575545585074480, -83.37298466334958391, -8.660254037844385522 ) ) ;
#7547 = AXIS2_PLACEMENT_3D ( 'NONE', #10243, #7783, #3048 ) ;
#7549 = DIRECTION ( 'NONE',  ( -0.1566598588826321192, 0.9876526153536342445, 7.798540720466730171E-17 ) ) ;
#7550 = CONICAL_SURFACE ( 'NONE', #9055, 12.74754878398196567, 0.01745329251994333364 ) ;
#7551 = DIRECTION ( 'NONE',  ( -0.1566598588826321747, 0.9876526153536343555, 0.000000000000000000 ) ) ;
#7552 = ORIENTED_EDGE ( 'NONE', *, *, #8475, .F. ) ;
#7553 = VERTEX_POINT ( 'NONE', #1563 ) ;
#7554 = DIRECTION ( 'NONE',  ( -0.9876526153536341335, -0.1566598588826327021, 0.000000000000000000 ) ) ;
#7555 = VECTOR ( 'NONE', #9728, 1000.000000000000000 ) ;
#7556 = AXIS2_PLACEMENT_3D ( 'NONE', #10219, #16008, #4536 ) ;
#7557 = AXIS2_PLACEMENT_3D ( 'NONE', #16454, #7821, #16535 ) ;
#7558 = ORIENTED_EDGE ( 'NONE', *, *, #14992, .T. ) ;
#7559 = EDGE_LOOP ( 'NONE', ( #10766, #14568, #1919, #8390 ) ) ;
#7560 = ORIENTED_EDGE ( 'NONE', *, *, #16132, .F. ) ;
#7561 = CIRCLE ( 'NONE', #6370, 1.500000000000000888 ) ;
#7562 = AXIS2_PLACEMENT_3D ( 'NONE', #13989, #12173, #5279 ) ;
#7563 = CIRCLE ( 'NONE', #6667, 1.500000000000000444 ) ;
#7564 = CARTESIAN_POINT ( 'NONE',  ( 73.09088021254186174, 1.387778780781445676E-14, -25.00000000000000000 ) ) ;
#7565 = AXIS2_PLACEMENT_3D ( 'NONE', #221, #5912, #17405 ) ;
#7566 = CARTESIAN_POINT ( 'NONE',  ( 0.000000000000000000, 0.000000000000000000, -24.99999999999999289 ) ) ;
#7567 = CARTESIAN_POINT ( 'NONE',  ( 0.4120860815263194254, -77.88988960245745830, 1.077796531449093893E-14 ) ) ;
#7568 = AXIS2_PLACEMENT_3D ( 'NONE', #6342, #12074, #9906 ) ;
#7569 = VERTEX_POINT ( 'NONE', #14626 ) ;
#7570 = DIRECTION ( 'NONE',  ( 0.000000000000000000, 0.000000000000000000, 1.000000000000000000 ) ) ;
#7571 = LINE ( 'NONE', #16193, #18161 ) ;
#7572 = DIRECTION ( 'NONE',  ( 0.000000000000000000, 0.000000000000000000, 1.000000000000000000 ) ) ;
#7573 = CIRCLE ( 'NONE', #14242, 1.499999999999999556 ) ;
#7574 = CARTESIAN_POINT ( 'NONE',  ( -35.67686938905902849, -25.90879301532540779, 12.99038105676661736 ) ) ;
#7575 = ORIENTED_EDGE ( 'NONE', *, *, #8063, .F. ) ;
#7576 = AXIS2_PLACEMENT_3D ( 'NONE', #18418, #5487, #9757 ) ;
#7578 = ORIENTED_EDGE ( 'NONE', *, *, #5855, .F. ) ;
#7577 = DIRECTION ( 'NONE',  ( -0.000000000000000000, -0.000000000000000000, 1.000000000000000000 ) ) ;
#7579 = ADVANCED_FACE ( 'NONE', ( #2862 ), #5731, .F. ) ;
#7580 = EDGE_LOOP ( 'NONE', ( #8468, #5016 ) ) ;
#7581 = AXIS2_PLACEMENT_3D ( 'NONE', #3232, #6109, #6399 ) ;
#7582 = ORIENTED_EDGE ( 'NONE', *, *, #7428, .F. ) ;
#7583 = ADVANCED_FACE ( 'NONE', ( #11383 ), #16046, .F. ) ;
#7584 = CARTESIAN_POINT ( 'NONE',  ( -39.09401853261887538, -84.15628395776273862, 17.32050807568881368 ) ) ;
#7585 = CIRCLE ( 'NONE', #13624, 1.500000000000000444 ) ;
#7586 = ORIENTED_EDGE ( 'NONE', *, *, #8928, .T. ) ;
#7587 = EDGE_LOOP ( 'NONE', ( #2758, #6560 ) ) ;
#7588 = CARTESIAN_POINT ( 'NONE',  ( -7.528769851480577202, -21.44398703717040888, -4.330127018922184767 ) ) ;
#7589 = CARTESIAN_POINT ( 'NONE',  ( -61.31620237807555895, -87.68113078262196325, 12.99038105676661203 ) ) ;
#7590 = AXIS2_PLACEMENT_3D ( 'NONE', #12155, #13860, #3717 ) ;
#7591 = DIRECTION ( 'NONE',  ( -0.9876526153536336894, -0.1566598588826349503, 0.000000000000000000 ) ) ;
#7592 = AXIS2_PLACEMENT_3D ( 'NONE', #5671, #11420, #17253 ) ;
#7593 = ORIENTED_EDGE ( 'NONE', *, *, #13938, .T. ) ;
#7594 = CARTESIAN_POINT ( 'NONE',  ( -46.50141314777111745, -85.33123289938248490, -4.330127018922185655 ) ) ;
#7595 = CIRCLE ( 'NONE', #18232, 1.500000000000001332 ) ;
#7596 = LINE ( 'NONE', #9103, #7819 ) ;
#7597 = DIRECTION ( 'NONE',  ( -0.1566598588826321192, 0.9876526153536342445, 7.798540720466730171E-17 ) ) ;
#7598 = DIRECTION ( 'NONE',  ( 0.000000000000000000, 0.000000000000000000, 1.000000000000000000 ) ) ;
#7599 = ORIENTED_EDGE ( 'NONE', *, *, #12705, .T. ) ;
#7600 = FACE_BOUND ( 'NONE', #5472, .T. ) ;
#7601 =( LENGTH_UNIT ( ) NAMED_UNIT ( * ) SI_UNIT ( .MILLI., .METRE. ) );
#7602 = ORIENTED_EDGE ( 'NONE', *, *, #12410, .T. ) ;
#7603 = CARTESIAN_POINT ( 'NONE',  ( -3.538524379888208227, -78.51652903798800764, 4.330127018922209636 ) ) ;
#7604 = VECTOR ( 'NONE', #3930, 1000.000000000000000 ) ;
#7605 = CARTESIAN_POINT ( 'NONE',  ( -56.21322099054477661, -24.10372711620991026, 12.99038105676661736 ) ) ;
#7606 = ORIENTED_EDGE ( 'NONE', *, *, #14706, .F. ) ;
#7607 = VECTOR ( 'NONE', #6600, 1000.000000000000000 ) ;
#7608 = VERTEX_POINT ( 'NONE', #1289 ) ;
#7609 = ORIENTED_EDGE ( 'NONE', *, *, #14943, .F. ) ;
#7610 = VERTEX_POINT ( 'NONE', #11574 ) ;
#7611 = DIRECTION ( 'NONE',  ( 1.000000000000000000, 0.000000000000000000, 0.000000000000000000 ) ) ;
#7612 = AXIS2_PLACEMENT_3D ( 'NONE', #5435, #6581, #15484 ) ;
#7613 = EDGE_CURVE ( 'NONE', #859, #14096, #7424, .T. ) ;
#7614 = FACE_BOUND ( 'NONE', #3688, .T. ) ;
#7615 = EDGE_LOOP ( 'NONE', ( #5587, #12165, #14385, #2233 ) ) ;
#7616 = CARTESIAN_POINT ( 'NONE',  ( -2.879979761448749009, -15.64409473654778893, 17.32050807568881012 ) ) ;
#7617 = ORIENTED_EDGE ( 'NONE', *, *, #9056, .F. ) ;
#7618 = ADVANCED_FACE ( 'NONE', ( #4084, #17481, #5831, #14257, #4384, #17312, #1374, #18663, #4471, #10251, #5631, #17209, #13181, #15771, #14535, #209, #2789, #8576, #14347, #4296, #10069, #7157, #15856, #4842, #11846, #6390, #4655, #3221, #9017, #6479, #498, #1724, #9122, #6195, #14989, #10709, #9296, #13650, #16430, #597, #17864, #11924, #16227, #3411, #16510, #13272, #3498, #13549, #3321, #10630, #12124, #1918, #13377, #15076, #2099, #7886, #9214, #2004, #17683, #7793, #694, #14708, #410, #17771, #17586, #17964, #10529, #4928, #4748, #4568, #7704, #16324, #10342, #7614, #1823, #14897, #16143, #3136, #8927, #7510, #308, #10434, #6100, #13456, #14800, #6292, #12020, #782, #5416, #12310, #2483, #3778, #9494, #989, #11175, #18054, #12511, #14032, #17003, #9581, #16715, #3870, #1171, #9696, #16812, #12214, #8167, #2278, #8272, #5233, #5323, #6760, #15358, #6565, #18352, #1079, #8061, #3594, #2374, #16608, #7975, #6663, #5015, #13837, #15261, #884, #3977, #10793, #6848, #2566, #15549, #9402, #13936, #15465, #11080, #16905, #15180, #5124, #14122, #8352, #12418, #12593, #18262, #18452, #10983, #9779, #18154, #2194, #13732, #10896, #3691, #1441, #11277, #9864, #15840, #7052, #11549, #6952, #4065, #4272, #17289, #8452, #11633, #7136, #12977, #17459, #14330, #5610, #17380, #5888, #2659, #4448, #2928, #11453, #17, #1536, #10050, #2768, #105, #10228, #16021, #5809 ), #14603, .F. ) ;
#7619 = CIRCLE ( 'NONE', #2474, 1.500000000000000888 ) ;
#7620 = CIRCLE ( 'NONE', #7911, 2.500000000000002220 ) ;
#7621 = EDGE_LOOP ( 'NONE', ( #3492, #8695, #4045, #4111, #13664 ) ) ;
#7622 = CARTESIAN_POINT ( 'NONE',  ( -70.00000000000001421, 44.99999999999998579, -7.500000000000000000 ) ) ;
#7623 = FACE_BOUND ( 'NONE', #4354, .T. ) ;
#7624 = AXIS2_PLACEMENT_3D ( 'NONE', #4047, #18338, #3955 ) ;
#7625 = FACE_OUTER_BOUND ( 'NONE', #13684, .T. ) ;
#7626 = DIRECTION ( 'NONE',  ( 1.000000000000000000, 0.000000000000000000, 0.000000000000000000 ) ) ;
#7627 = CIRCLE ( 'NONE', #7935, 2.500000000000002220 ) ;
#7628 = DIRECTION ( 'NONE',  ( -0.1615579233078772992, -0.9868632313631134911, 0.000000000000000000 ) ) ;
#7629 = CARTESIAN_POINT ( 'NONE',  ( -49.26481467677530901, 51.83848025225072575, -130.3485206753969976 ) ) ;
#7630 = ORIENTED_EDGE ( 'NONE', *, *, #3962, .T. ) ;
#7631 = ORIENTED_EDGE ( 'NONE', *, *, #17607, .T. ) ;
#7632 = CARTESIAN_POINT ( 'NONE',  ( -60.16383145195931803, -24.73036655174042409, -17.32050807568878170 ) ) ;
#7633 = CARTESIAN_POINT ( 'NONE',  ( -52.92115514756970640, -86.34952198211959740, 12.99038105676661203 ) ) ;
#7634 = CIRCLE ( 'NONE', #7923, 1.499999999999999556 ) ;
#7635 = EDGE_CURVE ( 'NONE', #7782, #4359, #2783, .T. ) ;
#7636 = VERTEX_POINT ( 'NONE', #15924 ) ;
#7637 = EDGE_LOOP ( 'NONE', ( #7115, #13195, #1185, #7799 ) ) ;
#7638 = LINE ( 'NONE', #1749, #3648 ) ;
#7639 = CARTESIAN_POINT ( 'NONE',  ( 6.831828081324923474, -76.87160051972034580, 1.096166233436304165E-14 ) ) ;
#7640 = AXIS2_PLACEMENT_3D ( 'NONE', #550, #1874, #4972 ) ;
#7641 = FACE_BOUND ( 'NONE', #1769, .T. ) ;
#7642 = EDGE_CURVE ( 'NONE', #1565, #10521, #10036, .T. ) ;
#7643 = DIRECTION ( 'NONE',  ( 0.000000000000000000, 0.000000000000000000, 1.000000000000000000 ) ) ;
#7644 = CARTESIAN_POINT ( 'NONE',  ( -2.000000000000000000, 0.000000000000000000, -24.99999999999999289 ) ) ;
#7645 = LINE ( 'NONE', #10559, #281 ) ;
#7646 = SURFACE_STYLE_FILL_AREA ( #7451 ) ;
#7647 = EDGE_LOOP ( 'NONE', ( #17634, #18658 ) ) ;
#7648 = VECTOR ( 'NONE', #16804, 1000.000000000000000 ) ;
#7649 = CARTESIAN_POINT ( 'NONE',  ( 55.85952145814821534, 6.938893903907228378E-15, 35.00000000000000000 ) ) ;
#7650 =( LENGTH_UNIT ( ) NAMED_UNIT ( * ) SI_UNIT ( .MILLI., .METRE. ) );
#7651 = LINE ( 'NONE', #12059, #4391 ) ;
#7652 = EDGE_LOOP ( 'NONE', ( #10797, #14956 ) ) ;
#7653 = ORIENTED_EDGE ( 'NONE', *, *, #3850, .F. ) ;
#7654 = VECTOR ( 'NONE', #9780, 1000.000000000000227 ) ;
#7655 = CARTESIAN_POINT ( 'NONE',  ( 7.819480696678544618, -76.71494066083772623, -21.65063509461098690 ) ) ;
#7656 = AXIS2_PLACEMENT_3D ( 'NONE', #17309, #8573, #7346 ) ;
#7657 = ORIENTED_EDGE ( 'NONE', *, *, #1882, .T. ) ;
#7658 = VERTEX_POINT ( 'NONE', #8554 ) ;
#7659 = EDGE_CURVE ( 'NONE', #14531, #17742, #14287, .T. ) ;
#7660 = ORIENTED_EDGE ( 'NONE', *, *, #5090, .T. ) ;
#7661 = ADVANCED_FACE ( 'NONE', ( #5521 ), #11364, .F. ) ;
#7662 = EDGE_CURVE ( 'NONE', #18009, #2581, #4594, .T. ) ;
#7663 = LINE ( 'NONE', #10576, #15953 ) ;
#7664 = EDGE_CURVE ( 'NONE', #16734, #17282, #7627, .T. ) ;
#7665 = AXIS2_PLACEMENT_3D ( 'NONE', #16413, #9195, #14965 ) ;
#7666 = ADVANCED_FACE ( 'NONE', ( #9950 ), #1356, .F. ) ;
#7667 = DIRECTION ( 'NONE',  ( -0.9876526153536336894, -0.1566598588826350336, 0.000000000000000000 ) ) ;
#7668 = ORIENTED_EDGE ( 'NONE', *, *, #16412, .T. ) ;
#7669 = DIRECTION ( 'NONE',  ( 3.816390434826605238E-17, 0.000000000000000000, -1.000000000000000000 ) ) ;
#7670 = FACE_OUTER_BOUND ( 'NONE', #7494, .T. ) ;
#7671 = CARTESIAN_POINT ( 'NONE',  ( -65.37641414873196766, 43.03264333350144710, 20.00000000000001066 ) ) ;
#7672 = ORIENTED_EDGE ( 'NONE', *, *, #13982, .F. ) ;
#7673 = DIRECTION ( 'NONE',  ( -0.1566598588826321192, 0.9876526153536342445, 7.798540720466730171E-17 ) ) ;
#7674 = DIRECTION ( 'NONE',  ( -0.1566598588826321192, 0.9876526153536342445, 7.798540720466730171E-17 ) ) ;
#7675 = DIRECTION ( 'NONE',  ( 0.000000000000000000, 0.000000000000000000, 1.000000000000000000 ) ) ;
#7677 = EDGE_LOOP ( 'NONE', ( #5582, #15521 ) ) ;
#7676 = CYLINDRICAL_SURFACE ( 'NONE', #10259, 1.500000000000001554 ) ;
#7678 = DIRECTION ( 'NONE',  ( -0.9876526153536341335, -0.1566598588826327021, 0.000000000000000000 ) ) ;
#7679 = ORIENTED_EDGE ( 'NONE', *, *, #11619, .F. ) ;
#7680 = ORIENTED_EDGE ( 'NONE', *, *, #2780, .T. ) ;
#7681 = CYLINDRICAL_SURFACE ( 'NONE', #15028, 1.500000000000001554 ) ;
#7682 = EDGE_CURVE ( 'NONE', #9201, #16508, #14414, .T. ) ;
#7683 = DIRECTION ( 'NONE',  ( -0.1566598588826321747, 0.9876526153536343555, 0.000000000000000000 ) ) ;
#7684 = VERTEX_POINT ( 'NONE', #10503 ) ;
#7685 = CARTESIAN_POINT ( 'NONE',  ( -16.91146969734005268, -22.93225569655540141, 8.660254037844417496 ) ) ;
#7686 = LINE ( 'NONE', #6607, #4699 ) ;
#7687 = CARTESIAN_POINT ( 'NONE',  ( 2.447859171744379392, -14.79900155049412014, -24.99999999999999289 ) ) ;
#7688 = EDGE_CURVE ( 'NONE', #15443, #2695, #10644, .T. ) ;
#7689 = EDGE_CURVE ( 'NONE', #3263, #4160, #1625, .T. ) ;
#7690 = AXIS2_PLACEMENT_3D ( 'NONE', #650, #6441, #5378 ) ;
#7691 = CARTESIAN_POINT ( 'NONE',  ( 2.000000000000000000, 2.449293598294706414E-16, 30.00000000000000000 ) ) ;
#7692 = CARTESIAN_POINT ( 'NONE',  ( -94.14047854185179176, 6.938893903907228378E-15, 35.00000000000000000 ) ) ;
#7693 = CARTESIAN_POINT ( 'NONE',  ( -1.892327146095128310, -15.48743487766515337, -21.65063509461097979 ) ) ;
#7694 = ORIENTED_EDGE ( 'NONE', *, *, #1068, .T. ) ;
#7695 = ORIENTED_EDGE ( 'NONE', *, *, #1576, .F. ) ;
#7696 = DIRECTION ( 'NONE',  ( -0.1566598588826321192, 0.9876526153536342445, 7.798540720466730171E-17 ) ) ;
#7697 = CARTESIAN_POINT ( 'NONE',  ( -31.52190560670403841, -20.18723064414412249, 21.65063509461102242 ) ) ;
#7698 = ORIENTED_EDGE ( 'NONE', *, *, #2195, .T. ) ;
#7699 = ORIENTED_EDGE ( 'NONE', *, *, #11873, .F. ) ;
#7700 = ORIENTED_EDGE ( 'NONE', *, *, #10985, .T. ) ;
#7701 = DIRECTION ( 'NONE',  ( 0.000000000000000000, 0.000000000000000000, 1.000000000000000000 ) ) ;
#7702 = VERTEX_POINT ( 'NONE', #9192 ) ;
#7703 = ORIENTED_EDGE ( 'NONE', *, *, #3123, .T. ) ;
#7704 = FACE_BOUND ( 'NONE', #15528, .T. ) ;
#7705 = VERTEX_POINT ( 'NONE', #13355 ) ;
#7706 = ORIENTED_EDGE ( 'NONE', *, *, #11389, .T. ) ;
#7707 = EDGE_CURVE ( 'NONE', #8225, #6018, #14876, .T. ) ;
#7708 = EDGE_CURVE ( 'NONE', #7294, #10326, #13433, .T. ) ;
#7709 = EDGE_LOOP ( 'NONE', ( #3086, #12853, #17911, #1032 ) ) ;
#7710 = CARTESIAN_POINT ( 'NONE',  ( -38.14600092744310444, -26.30044266253198160, 17.32050807568881723 ) ) ;
#7711 = ADVANCED_FACE ( 'NONE', ( #16488 ), #1801, .T. ) ;
#7712 = LINE ( 'NONE', #13658, #17297 ) ;
#7713 = CARTESIAN_POINT ( 'NONE',  ( -50.49165861936346289, -28.25869089856487903, 12.99038105676661736 ) ) ;
#7714 = DIRECTION ( 'NONE',  ( -0.9876526153536341335, -0.1566598588826327021, 0.000000000000000000 ) ) ;
#7715 = DIRECTION ( 'NONE',  ( -0.5989998693185459855, -0.8007491221077702725, -1.073713046591392860E-16 ) ) ;
#7716 = ORIENTED_EDGE ( 'NONE', *, *, #239, .F. ) ;
#7717 = ORIENTED_EDGE ( 'NONE', *, *, #8633, .F. ) ;
#7718 = CARTESIAN_POINT ( 'NONE',  ( -19.34096622554629263, -81.02308678011010556, -8.660254037844385522 ) ) ;
#7719 = VECTOR ( 'NONE', #7696, 1000.000000000000000 ) ;
#7720 = CYLINDRICAL_SURFACE ( 'NONE', #10869, 1.500000000000001554 ) ;
#7721 = CARTESIAN_POINT ( 'NONE',  ( -10.78120068427780964, -16.89737360760884144, 1.561251128379126385E-14 ) ) ;
#7722 = ORIENTED_EDGE ( 'NONE', *, *, #10438, .T. ) ;
#7723 = VERTEX_POINT ( 'NONE', #4638 ) ;
#7724 = LINE ( 'NONE', #13475, #10317 ) ;
#7725 = ORIENTED_EDGE ( 'NONE', *, *, #17460, .F. ) ;
#7726 = DIRECTION ( 'NONE',  ( 2.887450008416415878E-16, 0.000000000000000000, 1.000000000000000000 ) ) ;
#7727 = DIRECTION ( 'NONE',  ( 0.000000000000000000, 0.000000000000000000, 1.000000000000000000 ) ) ;
#7728 = SHAPE_REPRESENTATION_RELATIONSHIP ( 'NONE' , 'NONE' ,  #13127, #14079 ) ;
#7729 = EDGE_CURVE ( 'NONE', #8619, #3230, #13523, .T. ) ;
#7730 = CARTESIAN_POINT ( 'NONE',  ( -24.11451099155181055, -19.01228170252437266, -17.32050807568878170 ) ) ;
#7731 =( NAMED_UNIT ( * ) PLANE_ANGLE_UNIT ( ) SI_UNIT ( $, .RADIAN. ) );
#7732 = LINE ( 'NONE', #7924, #2869 ) ;
#7733 = ORIENTED_EDGE ( 'NONE', *, *, #11578, .T. ) ;
#7734 = ORIENTED_EDGE ( 'NONE', *, *, #12221, .F. ) ;
#7735 = LINE ( 'NONE', #10381, #15464 ) ;
#7736 = ORIENTED_EDGE ( 'NONE', *, *, #4207, .F. ) ;
#7737 = EDGE_CURVE ( 'NONE', #17224, #5271, #1585, .T. ) ;
#7738 = CARTESIAN_POINT ( 'NONE',  ( -55.22556837519115902, -23.94706725732727648, 8.660254037844417496 ) ) ;
#7739 = AXIS2_PLACEMENT_3D ( 'NONE', #138, #13013, #18761 ) ;
#7740 = ADVANCED_FACE ( 'NONE', ( #11904 ), #473, .F. ) ;
#7741 = EDGE_LOOP ( 'NONE', ( #9915, #17483 ) ) ;
#7742 = DIRECTION ( 'NONE',  ( 0.000000000000000000, 0.000000000000000000, 1.000000000000000000 ) ) ;
#7743 = FACE_OUTER_BOUND ( 'NONE', #13449, .T. ) ;
#7744 = ORIENTED_EDGE ( 'NONE', *, *, #10473, .F. ) ;
#7745 = LINE ( 'NONE', #11971, #18269 ) ;
#7746 = LINE ( 'NONE', #16191, #17240 ) ;
#7747 = DIRECTION ( 'NONE',  ( -0.000000000000000000, -0.000000000000000000, -1.000000000000000000 ) ) ;
#7748 = AXIS2_PLACEMENT_3D ( 'NONE', #14021, #2265, #9570 ) ;
#7749 = DIRECTION ( 'NONE',  ( 1.000000000000000000, 0.000000000000000000, 0.000000000000000000 ) ) ;
#7750 = ADVANCED_FACE ( 'NONE', ( #3118 ), #9094, .T. ) ;
#7751 = DIRECTION ( 'NONE',  ( -0.1566598588826321192, 0.9876526153536342445, 7.798540720466730171E-17 ) ) ;
#7752 = CARTESIAN_POINT ( 'NONE',  ( -70.00000000000000000, 44.99999999999999289, 110.7545852194966045 ) ) ;
#7753 = ADVANCED_FACE ( 'NONE', ( #17745 ), #3386, .F. ) ;
#7755 = ORIENTED_EDGE ( 'NONE', *, *, #18331, .T. ) ;
#7754 = CARTESIAN_POINT ( 'NONE',  ( -28.06512145296634486, -19.63892113805490425, 4.330127018922218518 ) ) ;
#7756 = EDGE_CURVE ( 'NONE', #18320, #11583, #12770, .T. ) ;
#7757 = CARTESIAN_POINT ( 'NONE',  ( -57.69469991357523497, -24.33871690453385739, 12.99038105676661736 ) ) ;
#7758 = CIRCLE ( 'NONE', #18402, 1.500000000000001332 ) ;
#7759 = VERTEX_POINT ( 'NONE', #7764 ) ;
#7760 = ORIENTED_EDGE ( 'NONE', *, *, #1940, .F. ) ;
#7761 = EDGE_LOOP ( 'NONE', ( #9860, #15009, #13900, #7224 ) ) ;
#7762 = DIRECTION ( 'NONE',  ( -0.9876526153536336894, -0.1566598588826349503, 0.000000000000000000 ) ) ;
#7763 = CIRCLE ( 'NONE', #16867, 1.499999999999999556 ) ;
#7764 = CARTESIAN_POINT ( 'NONE',  ( -74.48479437458692587, -27.00193450553858554, -21.65063509461098334 ) ) ;
#7765 = EDGE_LOOP ( 'NONE', ( #18473, #5462 ) ) ;
#7766 = LINE ( 'NONE', #6367, #1029 ) ;
#7767 = DIRECTION ( 'NONE',  ( -0.1566598588826321192, 0.9876526153536342445, 7.798540720466730171E-17 ) ) ;
#7768 = DIRECTION ( 'NONE',  ( -0.9876526153536336894, -0.1566598588826349503, 0.000000000000000000 ) ) ;
#7769 = PRODUCT_DEFINITION_CONTEXT ( 'detailed design', #3244, 'design' ) ;
#7770 = CIRCLE ( 'NONE', #11721, 2.999999999999999112 ) ;
#7771 = DIRECTION ( 'NONE',  ( 0.000000000000000000, -1.000000000000000000, 0.000000000000000000 ) ) ;
#7772 = CARTESIAN_POINT ( 'NONE',  ( -54.89646037827696290, -86.66284169988483654, -21.65063509461098690 ) ) ;
#7773 = DIRECTION ( 'NONE',  ( 0.000000000000000000, 0.000000000000000000, 1.000000000000000000 ) ) ;
#7774 = DIRECTION ( 'NONE',  ( -0.1566598588826321192, 0.9876526153536342445, 7.798540720466730171E-17 ) ) ;
#7775 = ORIENTED_EDGE ( 'NONE', *, *, #15544, .T. ) ;
#7776 = FACE_BOUND ( 'NONE', #8617, .T. ) ;
#7777 = EDGE_CURVE ( 'NONE', #11377, #1673, #4818, .T. ) ;
#7778 = FACE_OUTER_BOUND ( 'NONE', #5440, .T. ) ;
#7779 = ORIENTED_EDGE ( 'NONE', *, *, #15572, .T. ) ;
#7780 = DIRECTION ( 'NONE',  ( -0.9876526153536336894, -0.1566598588826349503, 0.000000000000000000 ) ) ;
#7781 = CIRCLE ( 'NONE', #10184, 1.500000000000000888 ) ;
#7782 = VERTEX_POINT ( 'NONE', #187 ) ;
#7783 = DIRECTION ( 'NONE',  ( -0.1566598588826321747, 0.9876526153536343555, 0.000000000000000000 ) ) ;
#7784 = CIRCLE ( 'NONE', #6571, 150.0000000000000284 ) ;
#7785 = ORIENTED_EDGE ( 'NONE', *, *, #16522, .T. ) ;
#7786 = ORIENTED_EDGE ( 'NONE', *, *, #15864, .F. ) ;
#7787 = LINE ( 'NONE', #5157, #1116 ) ;
#7788 = ORIENTED_EDGE ( 'NONE', *, *, #10748, .T. ) ;
#7789 = VERTEX_POINT ( 'NONE', #10694 ) ;
#7790 = DIRECTION ( 'NONE',  ( 0.000000000000000000, 0.000000000000000000, 1.000000000000000000 ) ) ;
#7791 = AXIS2_PLACEMENT_3D ( 'NONE', #14090, #16870, #12852 ) ;
#7792 = EDGE_LOOP ( 'NONE', ( #8504, #9735, #7938, #6146 ) ) ;
#7793 = FACE_BOUND ( 'NONE', #18424, .T. ) ;
#7794 = CARTESIAN_POINT ( 'NONE',  ( -14.23798483801550674, -17.44568311369805969, 1.908195823574487804E-14 ) ) ;
#7795 = ORIENTED_EDGE ( 'NONE', *, *, #14134, .F. ) ;
#7796 = CIRCLE ( 'NONE', #1745, 1.500000000000000000 ) ;
#7797 = VERTEX_POINT ( 'NONE', #570 ) ;
#7798 = FACE_BOUND ( 'NONE', #8065, .T. ) ;
#7799 = ORIENTED_EDGE ( 'NONE', *, *, #13175, .T. ) ;
#7800 = DIRECTION ( 'NONE',  ( 1.000000000000000000, 0.000000000000000000, -0.000000000000000000 ) ) ;
#7801 = DIRECTION ( 'NONE',  ( -0.9876526153536341335, -0.1566598588826327021, 0.000000000000000000 ) ) ;
#7802 = CARTESIAN_POINT ( 'NONE',  ( -172.7326993491721225, 43.83249341393818810, 9.951701414186830458E-16 ) ) ;
#7803 = CARTESIAN_POINT ( 'NONE',  ( -2.879979761448749009, -15.64409473654778893, -8.660254037844383745 ) ) ;
#7804 = CARTESIAN_POINT ( 'NONE',  ( -15.71946376104596155, -17.68067290202200326, -8.660254037844380193 ) ) ;
#7805 = ORIENTED_EDGE ( 'NONE', *, *, #5158, .F. ) ;
#7806 = VERTEX_POINT ( 'NONE', #12099 ) ;
#7807 = DIRECTION ( 'NONE',  ( -0.1566598588826321192, 0.9876526153536342445, 7.798540720466730171E-17 ) ) ;
#7808 = AXIS2_PLACEMENT_3D ( 'NONE', #10313, #3107, #2135 ) ;
#7809 = DIRECTION ( 'NONE',  ( -0.1566598588826321192, 0.9876526153536342445, 7.798540720466730171E-17 ) ) ;
#7810 = ADVANCED_FACE ( 'NONE', ( #6075 ), #4910, .F. ) ;
#7811 = CARTESIAN_POINT ( 'NONE',  ( 7.819480696678551723, -76.71494066083772623, 12.99038105676660493 ) ) ;
#7812 = ADVANCED_FACE ( 'NONE', ( #14686 ), #13161, .F. ) ;
#7813 = VERTEX_POINT ( 'NONE', #10870 ) ;
#7814 = LINE ( 'NONE', #12046, #14574 ) ;
#7815 = EDGE_LOOP ( 'NONE', ( #6142, #9440 ) ) ;
#7816 = EDGE_CURVE ( 'NONE', #56, #15303, #7864, .T. ) ;
#7817 = AXIS2_PLACEMENT_3D ( 'NONE', #6064, #6161, #3186 ) ;
#7818 = CARTESIAN_POINT ( 'NONE',  ( -61.31620237807555895, -87.68113078262193483, -21.65063509461098690 ) ) ;
#7819 = VECTOR ( 'NONE', #6082, 1000.000000000000000 ) ;
#7820 = AXIS2_PLACEMENT_3D ( 'NONE', #13769, #3533, #16197 ) ;
#7821 = DIRECTION ( 'NONE',  ( -0.1566598588826321192, 0.9876526153536342445, 7.798540720466731404E-17 ) ) ;
#7822 = CARTESIAN_POINT ( 'NONE',  ( -59.79999999999999716, 0.000000000000000000, 20.00000000000001776 ) ) ;
#7823 =( LENGTH_UNIT ( ) NAMED_UNIT ( * ) SI_UNIT ( .MILLI., .METRE. ) );
#7824 = CARTESIAN_POINT ( 'NONE',  ( -47.81817376003892406, -22.77211831570754441, 21.65063509461101887 ) ) ;
#7825 = DIRECTION ( 'NONE',  ( 0.000000000000000000, 0.000000000000000000, 1.000000000000000000 ) ) ;
#7826 = DIRECTION ( 'NONE',  ( -0.1566598588826321747, 0.9876526153536343555, 0.000000000000000000 ) ) ;
#7827 = DIRECTION ( 'NONE',  ( 1.000000000000000000, 0.000000000000000000, -0.000000000000000000 ) ) ;
#7828 = CARTESIAN_POINT ( 'NONE',  ( -80.30645961545690170, -27.92535762103353392, -24.99999999999999645 ) ) ;
#7829 = EDGE_LOOP ( 'NONE', ( #13753, #6310, #443, #14629 ) ) ;
#7830 = ORIENTED_EDGE ( 'NONE', *, *, #5814, .T. ) ;
#7831 = CARTESIAN_POINT ( 'NONE',  ( -15.22563745336913144, -17.60234297258069347, -4.330127018922180326 ) ) ;
#7832 = ORIENTED_EDGE ( 'NONE', *, *, #4294, .T. ) ;
#7833 = VECTOR ( 'NONE', #8625, 1000.000000000000000 ) ;
#7834 = AXIS2_PLACEMENT_3D ( 'NONE', #7802, #10716, #10446 ) ;
#7835 = ORIENTED_EDGE ( 'NONE', *, *, #3581, .F. ) ;
#7836 = EDGE_CURVE ( 'NONE', #8225, #827, #14300, .T. ) ;
#7837 = DIRECTION ( 'NONE',  ( -0.9876526153536341335, -0.1566598588826327021, 0.000000000000000000 ) ) ;
#7838 = DIRECTION ( 'NONE',  ( 0.000000000000000000, 0.000000000000000000, 1.000000000000000000 ) ) ;
#7839 = CIRCLE ( 'NONE', #2683, 1.500000000000001332 ) ;
#7840 = EDGE_LOOP ( 'NONE', ( #11882, #525 ) ) ;
#7841 = DIRECTION ( 'NONE',  ( 0.9826218788918644753, 0.1856185419698747896, 0.000000000000000000 ) ) ;
#7842 = AXIS2_PLACEMENT_3D ( 'NONE', #8568, #9792, #2855 ) ;
#7843 = EDGE_LOOP ( 'NONE', ( #7775, #10043 ) ) ;
#7844 = DIRECTION ( 'NONE',  ( -0.9868632313631133801, -0.1615579233078775490, 0.000000000000000000 ) ) ;
#7845 = EDGE_CURVE ( 'NONE', #299, #15709, #14014, .T. ) ;
#7846 = AXIS2_PLACEMENT_3D ( 'NONE', #2245, #10588, #16389 ) ;
#7847 = CARTESIAN_POINT ( 'NONE',  ( -46.33669483700850122, -22.53712852738357952, -21.65063509461097979 ) ) ;
#7848 = DIRECTION ( 'NONE',  ( -1.000000000000000000, 0.000000000000000000, 0.000000000000000000 ) ) ;
#7849 = CIRCLE ( 'NONE', #18496, 2.200000000000000178 ) ;
#7850 = CARTESIAN_POINT ( 'NONE',  ( -36.62488699423479943, -83.76463431055617548, 12.99038105676661203 ) ) ;
#7851 = CARTESIAN_POINT ( 'NONE',  ( -43.86756329862441817, -22.14547888017700217, -17.32050807568878170 ) ) ;
#7852 = ORIENTED_EDGE ( 'NONE', *, *, #11572, .F. ) ;
#7853 = CARTESIAN_POINT ( 'NONE',  ( -75.18297400320422241, -32.17518737063066681, -21.65063509461098334 ) ) ;
#7854 = EDGE_LOOP ( 'NONE', ( #1658, #9486, #17910, #1049 ) ) ;
#7855 = VECTOR ( 'NONE', #17401, 1000.000000000000000 ) ;
#7856 = DIRECTION ( 'NONE',  ( -0.9876526153536336894, -0.1566598588826350336, 0.000000000000000000 ) ) ;
#7857 = AXIS2_PLACEMENT_3D ( 'NONE', #1716, #7504, #1074 ) ;
#7858 = EDGE_LOOP ( 'NONE', ( #8234, #11548, #5747, #16182 ) ) ;
#7859 = VERTEX_POINT ( 'NONE', #2459 ) ;
#7860 = CIRCLE ( 'NONE', #12060, 1.500000000000000000 ) ;
#7861 = EDGE_CURVE ( 'NONE', #1673, #14356, #8555, .T. ) ;
#7862 = AXIS2_PLACEMENT_3D ( 'NONE', #14025, #9573, #9773 ) ;
#7863 = AXIS2_PLACEMENT_3D ( 'NONE', #8950, #15975, #15881 ) ;
#7864 = LINE ( 'NONE', #18430, #7053 ) ;
#7865 = DIRECTION ( 'NONE',  ( -0.9876526153536341335, -0.1566598588826327021, 0.000000000000000000 ) ) ;
#7866 = FACE_OUTER_BOUND ( 'NONE', #7637, .T. ) ;
#7867 = CARTESIAN_POINT ( 'NONE',  ( -69.99999999999998579, -45.00000000000000711, 25.00000000000000000 ) ) ;
#7868 = EDGE_CURVE ( 'NONE', #1312, #10401, #59, .T. ) ;
#7869 = VECTOR ( 'NONE', #12168, 1000.000000000000000 ) ;
#7870 = LINE ( 'NONE', #3678, #8726 ) ;
#7871 = VECTOR ( 'NONE', #2202, 1000.000000000000000 ) ;
#7872 = CARTESIAN_POINT ( 'NONE',  ( -39.09401853261890381, -84.15628395776272441, -17.32050807568878525 ) ) ;
#7873 = ORIENTED_EDGE ( 'NONE', *, *, #13364, .T. ) ;
#7874 = FACE_BOUND ( 'NONE', #7286, .T. ) ;
#7875 = VECTOR ( 'NONE', #5640, 1000.000000000000000 ) ;
#7876 = DIRECTION ( 'NONE',  ( 0.000000000000000000, 0.000000000000000000, -1.000000000000000000 ) ) ;
#7877 = CIRCLE ( 'NONE', #10887, 2.000000000000000000 ) ;
#7878 = CARTESIAN_POINT ( 'NONE',  ( -61.31620237807555895, -87.68113078262196325, 12.99038105676661203 ) ) ;
#7879 = PRODUCT_DEFINITION_SHAPE ( 'NONE', 'NONE',  #18796 ) ;
#7880 = VERTEX_POINT ( 'NONE', #9372 ) ;
#7881 = ORIENTED_EDGE ( 'NONE', *, *, #14833, .T. ) ;
#7882 = VECTOR ( 'NONE', #5493, 1000.000000000000000 ) ;
#7883 = ORIENTED_EDGE ( 'NONE', *, *, #9495, .F. ) ;
#7884 = ORIENTED_EDGE ( 'NONE', *, *, #101, .F. ) ;
#7885 = CARTESIAN_POINT ( 'NONE',  ( -24.81269062016910709, -24.18553456761645393, -17.32050807568878170 ) ) ;
#7886 = FACE_BOUND ( 'NONE', #1416, .T. ) ;
#7887 = EDGE_CURVE ( 'NONE', #17944, #6916, #17329, .T. ) ;
#7888 = AXIS2_PLACEMENT_3D ( 'NONE', #10143, #15931, #14521 ) ;
#7889 = EDGE_CURVE ( 'NONE', #12097, #3494, #18032, .T. ) ;
#7890 = ADVANCED_FACE ( 'NONE', ( #18126 ), #671, .F. ) ;
#7891 =( LENGTH_UNIT ( ) NAMED_UNIT ( * ) SI_UNIT ( .MILLI., .METRE. ) );
#7892 = CIRCLE ( 'NONE', #5476, 1.499999999999999556 ) ;
#7893 = CIRCLE ( 'NONE', #10302, 1.500000000000001332 ) ;
#7894 = DIRECTION ( 'NONE',  ( 0.000000000000000000, 0.000000000000000000, 1.000000000000000000 ) ) ;
#7895 = CIRCLE ( 'NONE', #3940, 1.500000000000000000 ) ;
#7896 = DIRECTION ( 'NONE',  ( -0.1566598588826321192, 0.9876526153536342445, 7.798540720466730171E-17 ) ) ;
#7897 = DIRECTION ( 'NONE',  ( -0.1566598588826321747, 0.9876526153536343555, 0.000000000000000000 ) ) ;
#7899 = CARTESIAN_POINT ( 'NONE',  ( -70.00000000000000000, 44.99999999999999289, 25.00000000000000000 ) ) ;
#7898 = AXIS2_PLACEMENT_3D ( 'NONE', #5777, #8614, #14386 ) ;
#7900 = CARTESIAN_POINT ( 'NONE',  ( 5.481473465377015408, 12.88229205725314408, 20.00000000000000000 ) ) ;
#7901 = FACE_OUTER_BOUND ( 'NONE', #1930, .T. ) ;
#7902 = VERTEX_POINT ( 'NONE', #858 ) ;
#7903 = ORIENTED_EDGE ( 'NONE', *, *, #13408, .F. ) ;
#7904 = CARTESIAN_POINT ( 'NONE',  ( -16.87183468716221313, -80.63143713290352821, -12.99038105676658539 ) ) ;
#7905 = CARTESIAN_POINT ( 'NONE',  ( -35.14340807120437660, -83.52964452223220349, -21.65063509461098690 ) ) ;
#7906 = DIRECTION ( 'NONE',  ( -0.1566598588826321192, 0.9876526153536342445, 7.798540720466730171E-17 ) ) ;
#7907 = VECTOR ( 'NONE', #5181, 1000.000000000000000 ) ;
#7908 = ORIENTED_EDGE ( 'NONE', *, *, #18226, .T. ) ;
#7909 = CARTESIAN_POINT ( 'NONE',  ( 0.000000000000000000, 0.000000000000000000, 25.00000000000000000 ) ) ;
#7910 = ORIENTED_EDGE ( 'NONE', *, *, #12350, .T. ) ;
#7911 = AXIS2_PLACEMENT_3D ( 'NONE', #1773, #6152, #16100 ) ;
#7912 = CARTESIAN_POINT ( 'NONE',  ( -169.9035932455946636, 31.96784544054909816, 3.719291248522914373 ) ) ;
#7913 = CARTESIAN_POINT ( 'NONE',  ( -173.9130733970031883, 56.16092972190472210, -3.146712427857100813 ) ) ;
#7914 = VERTEX_POINT ( 'NONE', #18236 ) ;
#7915 = DIRECTION ( 'NONE',  ( -0.1566598588826321192, 0.9876526153536342445, 7.798540720466730171E-17 ) ) ;
#7916 = AXIS2_PLACEMENT_3D ( 'NONE', #17843, #8045, #13811 ) ;
#7917 = FACE_OUTER_BOUND ( 'NONE', #1609, .T. ) ;
#7918 = ADVANCED_FACE ( 'NONE', ( #9468 ), #15442, .F. ) ;
#7919 = ORIENTED_EDGE ( 'NONE', *, *, #16789, .F. ) ;
#7920 = EDGE_CURVE ( 'NONE', #15461, #16941, #3851, .T. ) ;
#7921 = FACE_OUTER_BOUND ( 'NONE', #9971, .T. ) ;
#7922 = DIRECTION ( 'NONE',  ( -0.1566598588826321192, 0.9876526153536342445, 7.798540720466731404E-17 ) ) ;
#7923 = AXIS2_PLACEMENT_3D ( 'NONE', #46, #17403, #4386 ) ;
#7924 = CARTESIAN_POINT ( 'NONE',  ( -30.20514499443621759, -82.74634522781903456, -12.99038105676658539 ) ) ;
#7925 = CARTESIAN_POINT ( 'NONE',  ( -20.65772683781411345, -18.46397219643515797, -17.32050807568878170 ) ) ;
#7926 = VERTEX_POINT ( 'NONE', #13913 ) ;
#7927 = ORIENTED_EDGE ( 'NONE', *, *, #5488, .F. ) ;
#7928 = DIRECTION ( 'NONE',  ( 0.000000000000000000, 0.000000000000000000, 1.000000000000000000 ) ) ;
#7929 = VERTEX_POINT ( 'NONE', #10767 ) ;
#7930 = ORIENTED_EDGE ( 'NONE', *, *, #14580, .F. ) ;
#7931 = CIRCLE ( 'NONE', #18577, 1.500000000000000888 ) ;
#7932 = ORIENTED_EDGE ( 'NONE', *, *, #3193, .F. ) ;
#7933 = LINE ( 'NONE', #825, #17906 ) ;
#7934 = EDGE_LOOP ( 'NONE', ( #16899, #16526, #505, #18414 ) ) ;
#7935 = AXIS2_PLACEMENT_3D ( 'NONE', #15745, #10134, #4165 ) ;
#7936 = DIRECTION ( 'NONE',  ( -0.9876526153536341335, -0.1566598588826327021, 0.000000000000000000 ) ) ;
#7937 = DIRECTION ( 'NONE',  ( -0.1566598588826321192, 0.9876526153536342445, 7.798540720466730171E-17 ) ) ;
#7938 = ORIENTED_EDGE ( 'NONE', *, *, #7920, .T. ) ;
#7939 = AXIS2_PLACEMENT_3D ( 'NONE', #7499, #13444, #1547 ) ;
#7940 = CARTESIAN_POINT ( 'NONE',  ( -79.24244631363546887, 32.81909429640987952, 30.00000000000000000 ) ) ;
#7941 = DIRECTION ( 'NONE',  ( -0.1566598588826321192, 0.9876526153536342445, 7.798540720466730171E-17 ) ) ;
#7942 = CARTESIAN_POINT ( 'NONE',  ( -89.99999999999998579, -35.00000000000001421, 35.00000000000000000 ) ) ;
#7943 =( NAMED_UNIT ( * ) SI_UNIT ( $, .STERADIAN. ) SOLID_ANGLE_UNIT ( ) );
#7944 = EDGE_CURVE ( 'NONE', #4208, #7859, #17026, .T. ) ;
#7945 = CIRCLE ( 'NONE', #371, 1.499999999999999556 ) ;
#7946 = CARTESIAN_POINT ( 'NONE',  ( -30.73860631229088369, -25.12549372091224598, -4.330127018922181215 ) ) ;
#7947 = FACE_OUTER_BOUND ( 'NONE', #18518, .T. ) ;
#7948 = CARTESIAN_POINT ( 'NONE',  ( -2.057045456857760524, -78.28153924966404986, -4.330127018922185655 ) ) ;
#7949 = EDGE_CURVE ( 'NONE', #6894, #4082, #9751, .T. ) ;
#7951 = ORIENTED_EDGE ( 'NONE', *, *, #11122, .F. ) ;
#7950 = DIRECTION ( 'NONE',  ( -0.1566598588826321192, 0.9876526153536342445, 7.798540720466731404E-17 ) ) ;
#7952 = DIRECTION ( 'NONE',  ( -0.1566598588826321192, 0.9876526153536342445, 7.798540720466731404E-17 ) ) ;
#7953 = ORIENTED_EDGE ( 'NONE', *, *, #1331, .F. ) ;
#7954 = VERTEX_POINT ( 'NONE', #12571 ) ;
#7955 = DIRECTION ( 'NONE',  ( 0.000000000000000000, 0.000000000000000000, 1.000000000000000000 ) ) ;
#7956 = CARTESIAN_POINT ( 'NONE',  ( -44.03228160938702018, -84.93958325217590755, 17.32050807568881368 ) ) ;
#7957 = DIRECTION ( 'NONE',  ( -0.1566598588826321192, 0.9876526153536342445, 7.798540720466730171E-17 ) ) ;
#7958 = FACE_OUTER_BOUND ( 'NONE', #8301, .T. ) ;
#7959 = PLANE ( 'NONE',  #7239 ) ;
#7960 = DIRECTION ( 'NONE',  ( -0.1566598588826321192, 0.9876526153536342445, 7.798540720466730171E-17 ) ) ;
#7961 = DIRECTION ( 'NONE',  ( -0.1566598588826321192, 0.9876526153536342445, 7.798540720466731404E-17 ) ) ;
#7962 = VERTEX_POINT ( 'NONE', #13628 ) ;
#7963 = CARTESIAN_POINT ( 'NONE',  ( -40.08167114797249297, -84.31294381664537241, 21.65063509461101532 ) ) ;
#7964 = DIRECTION ( 'NONE',  ( -0.000000000000000000, -0.000000000000000000, -1.000000000000000000 ) ) ;
#7965 = VECTOR ( 'NONE', #1896, 1000.000000000000000 ) ;
#7966 = EDGE_CURVE ( 'NONE', #14612, #7022, #6458, .T. ) ;
#7967 = DIRECTION ( 'NONE',  ( -0.1566598588826321192, 0.9876526153536342445, 7.798540720466731404E-17 ) ) ;
#7968 = DIRECTION ( 'NONE',  ( -0.9876526153536336894, -0.1566598588826349503, 0.000000000000000000 ) ) ;
#7969 = ORIENTED_EDGE ( 'NONE', *, *, #17517, .F. ) ;
#7970 = EDGE_CURVE ( 'NONE', #4208, #13075, #3569, .T. ) ;
#7971 = VERTEX_POINT ( 'NONE', #2254 ) ;
#7972 = EDGE_LOOP ( 'NONE', ( #6396, #2762, #4444, #3305 ) ) ;
#7973 = DIRECTION ( 'NONE',  ( -1.000000000000000000, 0.000000000000000000, 0.000000000000000000 ) ) ;
#7974 = ADVANCED_FACE ( 'NONE', ( #16688 ), #13803, .T. ) ;
#7975 = FACE_BOUND ( 'NONE', #18012, .T. ) ;
#7976 = CIRCLE ( 'NONE', #12504, 1.500000000000000888 ) ;
#7977 = CARTESIAN_POINT ( 'NONE',  ( -30.69897130211303349, -82.82467515726035856, 7.308518362537324739E-15 ) ) ;
#7978 = SURFACE_STYLE_FILL_AREA ( #2196 ) ;
#7979 = ORIENTED_EDGE ( 'NONE', *, *, #220, .T. ) ;
#7980 = CARTESIAN_POINT ( 'NONE',  ( 2.000000000000000000, 2.449293598294706414E-16, -30.00000000000000000 ) ) ;
#7981 = CARTESIAN_POINT ( 'NONE',  ( -90.00000000000000000, 34.99999999999999289, 35.00000000000000000 ) ) ;
#7982 = ORIENTED_EDGE ( 'NONE', *, *, #16319, .F. ) ;
#7983 = LINE ( 'NONE', #16915, #17585 ) ;
#7984 = DIRECTION ( 'NONE',  ( -0.1566598588826321192, 0.9876526153536342445, 7.798540720466730171E-17 ) ) ;
#7985 = EDGE_CURVE ( 'NONE', #11183, #12777, #9127, .T. ) ;
#7986 = EDGE_LOOP ( 'NONE', ( #7903, #14982, #7310, #3419 ) ) ;
#7987 = ORIENTED_EDGE ( 'NONE', *, *, #14331, .F. ) ;
#7988 = CARTESIAN_POINT ( 'NONE',  ( -65.30644784966793281, -30.60858878180435738, -4.330127018922181215 ) ) ;
#7989 = EDGE_CURVE ( 'NONE', #18620, #8246, #5193, .T. ) ;
#7990 = EDGE_CURVE ( 'NONE', #9050, #12460, #12341, .T. ) ;
#7991 = DIRECTION ( 'NONE',  ( -0.1566598588826321192, 0.9876526153536342445, 7.798540720466731404E-17 ) ) ;
#7992 = VERTEX_POINT ( 'NONE', #15532 ) ;
#7993 = ORIENTED_EDGE ( 'NONE', *, *, #24, .T. ) ;
#7994 = CARTESIAN_POINT ( 'NONE',  ( 7.819480696678544618, -76.71494066083772623, -21.65063509461098690 ) ) ;
#7995 = EDGE_LOOP ( 'NONE', ( #8921, #8073, #5904, #3026 ) ) ;
#7996 = DIRECTION ( 'NONE',  ( -0.9876526153536341335, -0.1566598588826327021, 0.000000000000000000 ) ) ;
#7997 = CARTESIAN_POINT ( 'NONE',  ( -172.0951522251743029, 56.61964399677355431, -2.500000000000000000 ) ) ;
#7998 = EDGE_LOOP ( 'NONE', ( #759, #16404 ) ) ;
#7999 = CARTESIAN_POINT ( 'NONE',  ( -14.23798483801550674, -17.44568311369805613, -17.32050807568878170 ) ) ;
#8000 = DIRECTION ( 'NONE',  ( 0.000000000000000000, 0.000000000000000000, 1.000000000000000000 ) ) ;
#8001 = PRODUCT_CONTEXT ( 'NONE', #16966, 'mechanical' ) ;
#8002 = DIRECTION ( 'NONE',  ( 0.000000000000000000, 0.000000000000000000, 1.000000000000000000 ) ) ;
#8003 = CIRCLE ( 'NONE', #6824, 1.500000000000000888 ) ;
#8004 = SURFACE_SIDE_STYLE ('',( #2227 ) ) ;
#8005 = CARTESIAN_POINT ( 'NONE',  ( 3.133606229046292935, -19.12225244224100962, -24.99999999999999289 ) ) ;
#8006 = CARTESIAN_POINT ( 'NONE',  ( -77.72973689007648090, 30.96463005215034059, 35.00000000000000000 ) ) ;
#8007 = EDGE_CURVE ( 'NONE', #8907, #13690, #10024, .T. ) ;
#8008 = VERTEX_POINT ( 'NONE', #6925 ) ;
#8009 = ORIENTED_EDGE ( 'NONE', *, *, #14993, .F. ) ;
#8010 = CARTESIAN_POINT ( 'NONE',  ( -52.26261052913027072, -23.47708768067937513, -17.32050807568878170 ) ) ;
#8011 = ORIENTED_EDGE ( 'NONE', *, *, #8909, .T. ) ;
#8012 = PRODUCT_DEFINITION ( 'UNKNOWN', '', #18746, #14969 ) ;
#8013 = ORIENTED_EDGE ( 'NONE', *, *, #7104, .F. ) ;
#8014 = EDGE_CURVE ( 'NONE', #9857, #8644, #14867, .T. ) ;
#8015 = EDGE_CURVE ( 'NONE', #6018, #16818, #977, .T. ) ;
#8016 = AXIS2_PLACEMENT_3D ( 'NONE', #7375, #8688, #17345 ) ;
#8017 = CARTESIAN_POINT ( 'NONE',  ( -59.67000514428248437, -24.65203662229911430, -12.99038105676658006 ) ) ;
#8018 = DIRECTION ( 'NONE',  ( -0.1566598588826321192, 0.9876526153536342445, 7.798540720466731404E-17 ) ) ;
#8019 = VERTEX_POINT ( 'NONE', #8620 ) ;
#8020 = LINE ( 'NONE', #6811, #14345 ) ;
#8021 = DIRECTION ( 'NONE',  ( -1.000000000000000000, 0.000000000000000000, 0.000000000000000000 ) ) ;
#8022 = FILL_AREA_STYLE_COLOUR ( '', #3861 ) ;
#8023 = LINE ( 'NONE', #9257, #6021 ) ;
#8024 = DIRECTION ( 'NONE',  ( -0.1566598588826321192, 0.9876526153536342445, 7.798540720466730171E-17 ) ) ;
#8025 = FACE_BOUND ( 'NONE', #14692, .T. ) ;
#8026 = CARTESIAN_POINT ( 'NONE',  ( -19.34096622554629263, -81.02308678011010556, -8.660254037844385522 ) ) ;
#8027 = CARTESIAN_POINT ( 'NONE',  ( -81.61394393281571524, 30.50583143108602613, 35.00001199999999812 ) ) ;
#8028 = AXIS2_PLACEMENT_3D ( 'NONE', #324, #15087, #6304 ) ;
#8029 = ORIENTED_EDGE ( 'NONE', *, *, #8104, .T. ) ;
#8030 = DIRECTION ( 'NONE',  ( -0.9876526153536336894, -0.1566598588826350336, 0.000000000000000000 ) ) ;
#8031 = EDGE_LOOP ( 'NONE', ( #9835, #9736, #1763, #9465 ) ) ;
#8032 = ORIENTED_EDGE ( 'NONE', *, *, #9658, .F. ) ;
#8033 = EDGE_CURVE ( 'NONE', #4998, #11150, #5590, .T. ) ;
#8034 = ORIENTED_EDGE ( 'NONE', *, *, #16407, .T. ) ;
#8035 = ORIENTED_EDGE ( 'NONE', *, *, #4651, .F. ) ;
#8036 = EDGE_CURVE ( 'NONE', #10693, #241, #1276, .T. ) ;
#8037 = CIRCLE ( 'NONE', #12267, 1.500000000000000888 ) ;
#8038 = CARTESIAN_POINT ( 'NONE',  ( -3.538524379888211335, -78.51652903798800764, -21.65063509461098690 ) ) ;
#8039 = DIRECTION ( 'NONE',  ( -0.1566598588826321192, 0.9876526153536342445, 7.798540720466730171E-17 ) ) ;
#8040 = VERTEX_POINT ( 'NONE', #13051 ) ;
#8041 = EDGE_CURVE ( 'NONE', #11968, #12573, #14101, .T. ) ;
#8042 = CARTESIAN_POINT ( 'NONE',  ( -65.26681283949008616, -88.30777021815248418, 8.660254037844412167 ) ) ;
#8043 = CIRCLE ( 'NONE', #18698, 1.500000000000000444 ) ;
#8044 = ORIENTED_EDGE ( 'NONE', *, *, #15952, .F. ) ;
#8045 = DIRECTION ( 'NONE',  ( -0.1566598588826321747, 0.9876526153536343555, 0.000000000000000000 ) ) ;
#8046 = CARTESIAN_POINT ( 'NONE',  ( -19.17624791478365864, -18.22898240811121440, -17.32050807568878170 ) ) ;
#8047 = CARTESIAN_POINT ( 'NONE',  ( 0.000000000000000000, 0.000000000000000000, 25.00000000000000000 ) ) ;
#8048 = CARTESIAN_POINT ( 'NONE',  ( -76.17062661855784711, -32.33184722951329348, 1.887572821959364500E-14 ) ) ;
#8049 = ORIENTED_EDGE ( 'NONE', *, *, #6023, .F. ) ;
#8050 = DIRECTION ( 'NONE',  ( 0.000000000000000000, -1.445602896647339656E-16, 1.000000000000000000 ) ) ;
#8051 = DIRECTION ( 'NONE',  ( 0.000000000000000000, 0.000000000000000000, 1.000000000000000000 ) ) ;
#8052 = AXIS2_PLACEMENT_3D ( 'NONE', #17091, #16, #8637 ) ;
#8053 = CARTESIAN_POINT ( 'NONE',  ( -3.578159390066044665, -20.81734760163988440, -17.32050807568878170 ) ) ;
#8054 = CYLINDRICAL_SURFACE ( 'NONE', #18178, 1.500000000000001554 ) ;
#8055 = VERTEX_POINT ( 'NONE', #18526 ) ;
#8056 = CIRCLE ( 'NONE', #2302, 144.0000000000000284 ) ;
#8057 = ORIENTED_EDGE ( 'NONE', *, *, #1018, .T. ) ;
#8058 = ORIENTED_EDGE ( 'NONE', *, *, #8953, .F. ) ;
#8059 = VERTEX_POINT ( 'NONE', #11253 ) ;
#8060 = CARTESIAN_POINT ( 'NONE',  ( -60.32854976272193426, -87.52447092373932946, 17.32050807568881368 ) ) ;
#8061 = FACE_BOUND ( 'NONE', #7677, .T. ) ;
#8062 = AXIS2_PLACEMENT_3D ( 'NONE', #16126, #16204, #386 ) ;
#8063 = EDGE_CURVE ( 'NONE', #1063, #17245, #6724, .T. ) ;
#8064 =( GEOMETRIC_REPRESENTATION_CONTEXT ( 3 ) GLOBAL_UNCERTAINTY_ASSIGNED_CONTEXT ( ( #9101 ) ) GLOBAL_UNIT_ASSIGNED_CONTEXT ( ( #7650, #7731, #8955 ) ) REPRESENTATION_CONTEXT ( 'NONE', 'WORKASPACE' ) );
#8065 = EDGE_LOOP ( 'NONE', ( #11589, #4812 ) ) ;
#8066 = EDGE_CURVE ( 'NONE', #7806, #14381, #10636, .T. ) ;
#8067 = CARTESIAN_POINT ( 'NONE',  ( -69.99999999999998579, -45.00000000000000711, 110.7545852194966045 ) ) ;
#8068 = EDGE_LOOP ( 'NONE', ( #16852, #10719, #16686, #9216 ) ) ;
#8069 = EDGE_CURVE ( 'NONE', #3169, #1267, #17074, .T. ) ;
#8070 = CARTESIAN_POINT ( 'NONE',  ( 5.481473465377026955, -12.88229205725314763, -25.00000000000000000 ) ) ;
#8071 = CARTESIAN_POINT ( 'NONE',  ( -70.00000000000000000, 44.99999999999999289, -19.99999999999999645 ) ) ;
#8072 = CIRCLE ( 'NONE', #10194, 1.500000000000000888 ) ;
#8073 = ORIENTED_EDGE ( 'NONE', *, *, #11006, .T. ) ;
#8074 = ORIENTED_EDGE ( 'NONE', *, *, #18344, .F. ) ;
#8075 = DIRECTION ( 'NONE',  ( -0.1566598588826321192, 0.9876526153536342445, 7.798540720466730171E-17 ) ) ;
#8076 = CARTESIAN_POINT ( 'NONE',  ( 2.841582609732560272, -19.79905851890276836, -17.32050807568878170 ) ) ;
#8077 = CARTESIAN_POINT ( 'NONE',  ( -32.67427653282028643, -83.13799487502562613, -8.660254037844385522 ) ) ;
#8078 = ORIENTED_EDGE ( 'NONE', *, *, #10037, .F. ) ;
#8079 = ORIENTED_EDGE ( 'NONE', *, *, #11202, .T. ) ;
#8080 = CARTESIAN_POINT ( 'NONE',  ( -31.68662391746665463, -82.98133501614300656, 12.99038105676661203 ) ) ;
#8081 = AXIS2_PLACEMENT_3D ( 'NONE', #14546, #7261, #8381 ) ;
#8082 = PRESENTATION_LAYER_ASSIGNMENT (  '', '', ( #16262 ) ) ;
#8083 = CARTESIAN_POINT ( 'NONE',  ( -65.10209452872746283, -25.51366584615358946, 1.908195823574487804E-14 ) ) ;
#8084 = CIRCLE ( 'NONE', #10783, 2.200000000000000622 ) ;
#8085 = DIRECTION ( 'NONE',  ( -0.9876526153536336894, -0.1566598588826349503, 0.000000000000000000 ) ) ;
#8086 = AXIS2_PLACEMENT_3D ( 'NONE', #7527, #4763, #4666 ) ;
#8087 = DIRECTION ( 'NONE',  ( 0.000000000000000000, 0.000000000000000000, 1.000000000000000000 ) ) ;
#8088 = EDGE_CURVE ( 'NONE', #8327, #18200, #1421, .T. ) ;
#8089 = DIRECTION ( 'NONE',  ( -0.1566598588826321747, 0.9876526153536343555, 0.000000000000000000 ) ) ;
#8090 = DIRECTION ( 'NONE',  ( 0.000000000000000000, 0.000000000000000000, 1.000000000000000000 ) ) ;
#8091 = CARTESIAN_POINT ( 'NONE',  ( -34.15575545585074480, -83.37298466334958391, -17.32050807568878525 ) ) ;
#8092 = DIRECTION ( 'NONE',  ( 0.000000000000000000, 0.000000000000000000, 1.000000000000000000 ) ) ;
#8093 = ADVANCED_FACE ( 'NONE', ( #18709 ), #8422, .F. ) ;
#8094 = CARTESIAN_POINT ( 'NONE',  ( -77.72973689007648090, 30.96463005215034059, -30.00000000000000355 ) ) ;
#8095 = LINE ( 'NONE', #8300, #2025 ) ;
#8096 = PRODUCT_DEFINITION_FORMATION_WITH_SPECIFIED_SOURCE ( 'ANY', '', #12080, .NOT_KNOWN. ) ;
#8097 = AXIS2_PLACEMENT_3D ( 'NONE', #14456, #12835, #14553 ) ;
#8098 = DIRECTION ( 'NONE',  ( -0.9876526153536341335, -0.1566598588826327021, 0.000000000000000000 ) ) ;
#8099 = CARTESIAN_POINT ( 'NONE',  ( -94.14047854185179176, -35.00000000000001421, -30.00000000000000355 ) ) ;
#8100 = DIRECTION ( 'NONE',  ( -0.9876526153536336894, -0.1566598588826349503, 0.000000000000000000 ) ) ;
#8101 = ORIENTED_EDGE ( 'NONE', *, *, #11264, .T. ) ;
#8102 = ORIENTED_EDGE ( 'NONE', *, *, #16946, .T. ) ;
#8103 = APPLICATION_CONTEXT ( 'automotive_design' ) ;
#8104 = EDGE_CURVE ( 'NONE', #12986, #15683, #4044, .T. ) ;
#8105 = DIRECTION ( 'NONE',  ( -0.9876526153536341335, -0.1566598588826327021, 0.000000000000000000 ) ) ;
#8106 = CARTESIAN_POINT ( 'NONE',  ( -14.23798483801550674, -17.44568311369805969, 8.660254037844413944 ) ) ;
#8107 = EDGE_LOOP ( 'NONE', ( #16809, #10960, #5213, #10347 ) ) ;
#8108 = EDGE_LOOP ( 'NONE', ( #13930, #11217, #10573, #1876, #5779, #12069, #15785, #1476, #17897 ) ) ;
#8109 = CIRCLE ( 'NONE', #18753, 1.500000000000001332 ) ;
#8110 = CARTESIAN_POINT ( 'NONE',  ( -37.94164760650263446, -21.20551972688121722, -4.330127018922180326 ) ) ;
#8111 = ORIENTED_EDGE ( 'NONE', *, *, #17511, .F. ) ;
#8112 = ORIENTED_EDGE ( 'NONE', *, *, #1298, .T. ) ;
#8113 = DIRECTION ( 'NONE',  ( -0.1566598588826321192, 0.9876526153536342445, 7.798540720466730171E-17 ) ) ;
#8114 = DIRECTION ( 'NONE',  ( -0.1566598588826321747, 0.9876526153536343555, 0.000000000000000000 ) ) ;
#8115 = CIRCLE ( 'NONE', #17563, 12.83663829214476060 ) ;
#8116 = DIRECTION ( 'NONE',  ( -0.9876526153536336894, -0.1566598588826349503, 0.000000000000000000 ) ) ;
#8117 = CARTESIAN_POINT ( 'NONE',  ( -62.13913668266656032, -25.04368626950569166, -17.32050807568878170 ) ) ;
#8118 = EDGE_CURVE ( 'NONE', #5059, #5250, #2635, .T. ) ;
#8119 = AXIS2_PLACEMENT_3D ( 'NONE', #2355, #6743, #8148 ) ;
#8120 = ORIENTED_EDGE ( 'NONE', *, *, #5322, .F. ) ;
#8121 = EDGE_CURVE ( 'NONE', #1541, #18619, #17356, .T. ) ;
#8122 = CYLINDRICAL_SURFACE ( 'NONE', #6678, 1.500000000000001554 ) ;
#8123 = VERTEX_POINT ( 'NONE', #11612 ) ;
#8124 = CARTESIAN_POINT ( 'NONE',  ( -174.8673125818257006, 55.13264502119463373, 5.500000000000001776 ) ) ;
#8125 = DIRECTION ( 'NONE',  ( -0.9876526153536336894, -0.1566598588826350336, 0.000000000000000000 ) ) ;
#8126 = CARTESIAN_POINT ( 'NONE',  ( -48.97054468615519340, -85.72288254658904805, -8.660254037844385522 ) ) ;
#8128 = DIRECTION ( 'NONE',  ( -0.1566598588826321192, 0.9876526153536342445, 7.798540720466730171E-17 ) ) ;
#8127 = CIRCLE ( 'NONE', #18145, 1.500000000000000444 ) ;
#8129 = CIRCLE ( 'NONE', #16606, 145.0000000000000284 ) ;
#8130 = CARTESIAN_POINT ( 'NONE',  ( -4.565812005419673802, -20.97400746052251108, 21.65063509461101177 ) ) ;
#8131 = CARTESIAN_POINT ( 'NONE',  ( -84.08787250788334688, 32.13287136044273495, 35.00001199999999812 ) ) ;
#8132 = CIRCLE ( 'NONE', #7241, 1.500000000000000888 ) ;
#8134 = VERTEX_POINT ( 'NONE', #15712 ) ;
#8133 = DIRECTION ( 'NONE',  ( -0.9876526153536344665, -0.1566598588826304539, 0.000000000000000000 ) ) ;
#8135 = CARTESIAN_POINT ( 'NONE',  ( -33.20773785067495254, -25.51714336811882688, 1.869203119972154228E-14 ) ) ;
#8136 = CARTESIAN_POINT ( 'NONE',  ( -41.56315007100297265, -84.54793360496931598, -21.65063509461098690 ) ) ;
#8137 = ORIENTED_EDGE ( 'NONE', *, *, #7303, .T. ) ;
#8138 = ORIENTED_EDGE ( 'NONE', *, *, #2111, .F. ) ;
#8139 = VECTOR ( 'NONE', #8827, 1000.000000000000227 ) ;
#8140 = AXIS2_PLACEMENT_3D ( 'NONE', #14244, #9966, #12812 ) ;
#8141 = CARTESIAN_POINT ( 'NONE',  ( -13.45468554360235203, -22.38394619046619383, 17.32050807568881012 ) ) ;
#8142 = AXIS2_PLACEMENT_3D ( 'NONE', #5405, #5308, #16891 ) ;
#8143 = FACE_OUTER_BOUND ( 'NONE', #497, .T. ) ;
#8144 = DIRECTION ( 'NONE',  ( -0.1566598588826321747, 0.9876526153536343555, 0.000000000000000000 ) ) ;
#8145 = CIRCLE ( 'NONE', #7556, 1.500000000000000888 ) ;
#8146 = ORIENTED_EDGE ( 'NONE', *, *, #1580, .F. ) ;
#8147 = CARTESIAN_POINT ( 'NONE',  ( 0.000000000000000000, 0.000000000000000000, -35.00000000000000000 ) ) ;
#8148 = DIRECTION ( 'NONE',  ( -0.9876526153536336894, -0.1566598588826350336, 0.000000000000000000 ) ) ;
#8149 = CYLINDRICAL_SURFACE ( 'NONE', #889, 1.500000000000001554 ) ;
#8150 = DIRECTION ( 'NONE',  ( -0.1566598588826321192, 0.9876526153536342445, 7.798540720466730171E-17 ) ) ;
#8151 = DIRECTION ( 'NONE',  ( 0.1856185419698760941, -0.9826218788918640312, 0.000000000000000000 ) ) ;
#8152 = CARTESIAN_POINT ( 'NONE',  ( -27.57129514528951120, -19.56059120861359446, 8.660254037844417496 ) ) ;
#8153 = ORIENTED_EDGE ( 'NONE', *, *, #6391, .F. ) ;
#8154 = EDGE_CURVE ( 'NONE', #999, #334, #7619, .T. ) ;
#8155 = CIRCLE ( 'NONE', #11165, 1.500000000000000888 ) ;
#8156 = EDGE_CURVE ( 'NONE', #13974, #2654, #14279, .T. ) ;
#8157 = FACE_OUTER_BOUND ( 'NONE', #14229, .T. ) ;
#8158 = CARTESIAN_POINT ( 'NONE',  ( -63.62061560569699736, -25.27867605782964944, 17.32050807568882078 ) ) ;
#8159 = VECTOR ( 'NONE', #18348, 1000.000000000000000 ) ;
#8160 = VECTOR ( 'NONE', #6135, 1000.000000000000000 ) ;
#8161 = DIRECTION ( 'NONE',  ( 0.000000000000000000, 0.000000000000000000, 1.000000000000000000 ) ) ;
#8162 = VECTOR ( 'NONE', #12677, 1000.000000000000114 ) ;
#8163 = AXIS2_PLACEMENT_3D ( 'NONE', #11505, #5766, #5851 ) ;
#8164 = EDGE_LOOP ( 'NONE', ( #5141, #16798 ) ) ;
#8165 = EDGE_LOOP ( 'NONE', ( #14904, #16483, #14594, #15128, #6474, #8178 ) ) ;
#8166 = DIRECTION ( 'NONE',  ( -0.1566598588826321192, 0.9876526153536342445, 7.798540720466730171E-17 ) ) ;
#8167 = FACE_BOUND ( 'NONE', #12601, .T. ) ;
#8168 = AXIS2_PLACEMENT_3D ( 'NONE', #14055, #14154, #1196 ) ;
#8169 = CIRCLE ( 'NONE', #5765, 150.0000000000000000 ) ;
#8170 = EDGE_LOOP ( 'NONE', ( #6969, #11492, #1562, #3336 ) ) ;
#8171 = AXIS2_PLACEMENT_3D ( 'NONE', #13866, #11212, #5262 ) ;
#8172 = CIRCLE ( 'NONE', #12, 3.000000000000000888 ) ;
#8173 = CARTESIAN_POINT ( 'NONE',  ( -13.45468554360235203, -22.38394619046619383, 8.660254037844413944 ) ) ;
#8174 = CARTESIAN_POINT ( 'NONE',  ( -306.1404785418517918, -2.850701963179328668, 9.951701414186818625E-16 ) ) ;
#8175 = EDGE_LOOP ( 'NONE', ( #6041, #184, #1929, #15160 ) ) ;
#8176 = DIRECTION ( 'NONE',  ( -0.9876526153536341335, -0.1566598588826327021, 0.000000000000000000 ) ) ;
#8177 = CARTESIAN_POINT ( 'NONE',  ( 5.481473465377026955, -12.88229205725314763, 25.00000000000000000 ) ) ;
#8178 = ORIENTED_EDGE ( 'NONE', *, *, #12910, .F. ) ;
#8179 = DIRECTION ( 'NONE',  ( 0.000000000000000000, 0.000000000000000000, 1.000000000000000000 ) ) ;
#8180 = DIRECTION ( 'NONE',  ( -0.1566598588826321192, 0.9876526153536342445, 7.798540720466730171E-17 ) ) ;
#8181 = DIRECTION ( 'NONE',  ( -0.9876526153536336894, -0.1566598588826349503, 0.000000000000000000 ) ) ;
#8182 = ORIENTED_EDGE ( 'NONE', *, *, #5810, .F. ) ;
#8183 = DIRECTION ( 'NONE',  ( -0.1566598588826321192, 0.9876526153536342445, 7.798540720466730171E-17 ) ) ;
#8184 = EDGE_CURVE ( 'NONE', #8789, #5011, #11699, .T. ) ;
#8185 = CARTESIAN_POINT ( 'NONE',  ( -67.77557938805200877, -31.00023842901093118, 8.660254037844417496 ) ) ;
#8186 = AXIS2_PLACEMENT_3D ( 'NONE', #7020, #18516, #6624 ) ;
#8187 = DIRECTION ( 'NONE',  ( -0.9876526153536341335, -0.1566598588826327021, 0.000000000000000000 ) ) ;
#8188 = ORIENTED_EDGE ( 'NONE', *, *, #2521, .F. ) ;
#8189 = ORIENTED_EDGE ( 'NONE', *, *, #1377, .F. ) ;
#8190 = AXIS2_PLACEMENT_3D ( 'NONE', #10993, #6675, #12518 ) ;
#8191 = DIRECTION ( 'NONE',  ( -0.1566598588826321192, 0.9876526153536342445, 7.798540720466730171E-17 ) ) ;
#8192 = CYLINDRICAL_SURFACE ( 'NONE', #666, 1.500000000000001554 ) ;
#8193 = EDGE_CURVE ( 'NONE', #1545, #4233, #13052, .T. ) ;
#8194 = DIRECTION ( 'NONE',  ( -0.9876526153536341335, -0.1566598588826327021, 0.000000000000000000 ) ) ;
#8195 = VECTOR ( 'NONE', #3620, 1000.000000000000000 ) ;
#8196 = CARTESIAN_POINT ( 'NONE',  ( -52.75643683680708307, -23.55541761012069202, -4.330127018922180326 ) ) ;
#8197 = AXIS2_PLACEMENT_3D ( 'NONE', #6141, #10469, #16266 ) ;
#8198 = LINE ( 'NONE', #13967, #8483 ) ;
#8199 = DIRECTION ( 'NONE',  ( -0.9876526153536341335, -0.1566598588826327021, 0.000000000000000000 ) ) ;
#8200 = CARTESIAN_POINT ( 'NONE',  ( 4.210882526620689958, 82.14568124701358443, -2.815437546184208717 ) ) ;
#8201 = CARTESIAN_POINT ( 'NONE',  ( 3.231158466157551423, 19.73726462726227737, -35.00000000000000000 ) ) ;
#8202 = CARTESIAN_POINT ( 'NONE',  ( -15.22563745336913144, -17.60234297258068636, -21.65063509461098334 ) ) ;
#8203 = ORIENTED_EDGE ( 'NONE', *, *, #15252, .F. ) ;
#8204 = AXIS2_PLACEMENT_3D ( 'NONE', #10942, #6606, #15312 ) ;
#8205 = DIRECTION ( 'NONE',  ( -0.1566598588826321192, 0.9876526153536342445, 7.798540720466731404E-17 ) ) ;
#8206 = ORIENTED_EDGE ( 'NONE', *, *, #6482, .T. ) ;
#8207 = VERTEX_POINT ( 'NONE', #10199 ) ;
#8208 = DIRECTION ( 'NONE',  ( -0.9876526153536341335, -0.1566598588826327021, 0.000000000000000000 ) ) ;
#8209 = EDGE_CURVE ( 'NONE', #5983, #3731, #7337, .T. ) ;
#8210 = ORIENTED_EDGE ( 'NONE', *, *, #12297, .F. ) ;
#8211 = VECTOR ( 'NONE', #11480, 1000.000000000000000 ) ;
#8212 = ORIENTED_EDGE ( 'NONE', *, *, #17684, .T. ) ;
#8213 = AXIS2_PLACEMENT_3D ( 'NONE', #11220, #12254, #18203 ) ;
#8214 = VERTEX_POINT ( 'NONE', #545 ) ;
#8215 = DIRECTION ( 'NONE',  ( -0.9876526153536341335, -0.1566598588826327021, 0.000000000000000000 ) ) ;
#8216 = EDGE_CURVE ( 'NONE', #5889, #897, #14576, .T. ) ;
#8217 = AXIS2_PLACEMENT_3D ( 'NONE', #12645, #18505, #8316 ) ;
#8218 = DIRECTION ( 'NONE',  ( -0.9876526153536336894, -0.1566598588826350336, 0.000000000000000000 ) ) ;
#8219 = ORIENTED_EDGE ( 'NONE', *, *, #16094, .T. ) ;
#8220 = DIRECTION ( 'NONE',  ( -0.9876526153536336894, -0.1566598588826349503, 0.000000000000000000 ) ) ;
#8221 = DIRECTION ( 'NONE',  ( -0.9876526153536341335, -0.1566598588826327576, 0.000000000000000000 ) ) ;
#8222 = DIRECTION ( 'NONE',  ( 0.000000000000000000, 0.000000000000000000, -1.000000000000000000 ) ) ;
#8223 = DIRECTION ( 'NONE',  ( 0.000000000000000000, 0.000000000000000000, 1.000000000000000000 ) ) ;
#8224 = AXIS2_PLACEMENT_3D ( 'NONE', #5497, #15820, #9844 ) ;
#8225 = VERTEX_POINT ( 'NONE', #4422 ) ;
#8226 = ORIENTED_EDGE ( 'NONE', *, *, #6239, .F. ) ;
#8227 = CIRCLE ( 'NONE', #12127, 1.500000000000001332 ) ;
#8228 = APPLICATION_CONTEXT ( 'automotive_design' ) ;
#8229 = DIRECTION ( 'NONE',  ( -0.9876526153536341335, -0.1566598588826327021, 0.000000000000000000 ) ) ;
#8230 = VERTEX_POINT ( 'NONE', #11795 ) ;
#8231 = EDGE_CURVE ( 'NONE', #10127, #6097, #527, .T. ) ;
#8232 = CYLINDRICAL_SURFACE ( 'NONE', #18090, 1.500000000000001554 ) ;
#8233 = CARTESIAN_POINT ( 'NONE',  ( -49.59961335071795929, 37.20051552679455398, 20.00000000000001066 ) ) ;
#8234 = ORIENTED_EDGE ( 'NONE', *, *, #18226, .F. ) ;
#8235 = CIRCLE ( 'NONE', #12449, 20.00000000000001066 ) ;
#8236 = CARTESIAN_POINT ( 'NONE',  ( -129.1404785418517918, -15.35070196317932911, -5.500000000000000000 ) ) ;
#8237 = CARTESIAN_POINT ( 'NONE',  ( -6.007655918272284623, -78.90817868519457079, 1.424741226644455312E-14 ) ) ;
#8238 = ORIENTED_EDGE ( 'NONE', *, *, #11575, .T. ) ;
#8239 = AXIS2_PLACEMENT_3D ( 'NONE', #2846, #15633, #17093 ) ;
#8240 = EDGE_CURVE ( 'NONE', #5485, #3473, #6898, .T. ) ;
#8241 = DIRECTION ( 'NONE',  ( -2.671473304378624222E-16, -0.000000000000000000, -1.000000000000000000 ) ) ;
#8242 = EDGE_CURVE ( 'NONE', #4549, #12880, #4612, .T. ) ;
#8243 = CARTESIAN_POINT ( 'NONE',  ( -11.93357161039406300, -79.84813783849035929, -21.65063509461098690 ) ) ;
#8244 = ORIENTED_EDGE ( 'NONE', *, *, #9562, .T. ) ;
#8245 = EDGE_CURVE ( 'NONE', #442, #6801, #11690, .T. ) ;
#8246 = VERTEX_POINT ( 'NONE', #13138 ) ;
#8247 = CIRCLE ( 'NONE', #4307, 1.500000000000000888 ) ;
#8248 = CARTESIAN_POINT ( 'NONE',  ( 0.3724510713484854851, -20.19070816610934926, 4.330127018922212301 ) ) ;
#8249 = CARTESIAN_POINT ( 'NONE',  ( -46.50141314777111745, -85.33123289938247069, -12.99038105676658539 ) ) ;
#8250 = EDGE_CURVE ( 'NONE', #10116, #13151, #216, .T. ) ;
#8251 = VERTEX_POINT ( 'NONE', #168 ) ;
#8252 = DIRECTION ( 'NONE',  ( -1.000000000000000000, 0.000000000000000000, 0.000000000000000000 ) ) ;
#8253 = DIRECTION ( 'NONE',  ( 0.000000000000000000, -1.000000000000000000, 0.000000000000000000 ) ) ;
#8254 = DIRECTION ( 'NONE',  ( -0.1566598588826321192, 0.9876526153536342445, 7.798540720466731404E-17 ) ) ;
#8255 = DIRECTION ( 'NONE',  ( -0.1566598588826321747, 0.9876526153536343555, 0.000000000000000000 ) ) ;
#8256 = CARTESIAN_POINT ( 'NONE',  ( -40.61513246582718750, -26.69209230973856251, -12.99038105676658006 ) ) ;
#8257 = EDGE_LOOP ( 'NONE', ( #7606, #13871 ) ) ;
#8258 = DIRECTION ( 'NONE',  ( -0.1566598588826321192, 0.9876526153536342445, 7.798540720466730171E-17 ) ) ;
#8259 = AXIS2_PLACEMENT_3D ( 'NONE', #14318, #12787, #5600 ) ;
#8260 = CARTESIAN_POINT ( 'NONE',  ( -70.00000000000000000, 44.99999999999999289, -19.99999999999998934 ) ) ;
#8261 = CARTESIAN_POINT ( 'NONE',  ( -79.13358446461874962, -32.80182680616118773, -8.660254037844380193 ) ) ;
#8262 = EDGE_CURVE ( 'NONE', #1456, #2063, #7663, .T. ) ;
#8264 = EDGE_LOOP ( 'NONE', ( #15990, #13116, #14199, #7694 ) ) ;
#8263 = EDGE_CURVE ( 'NONE', #6009, #14985, #9591, .T. ) ;
#8265 = CARTESIAN_POINT ( 'NONE',  ( -53.94844277310118486, -28.80700040465408662, -12.99038105676658006 ) ) ;
#8266 = AXIS2_PLACEMENT_3D ( 'NONE', #12978, #5976, #14233 ) ;
#8267 = ORIENTED_EDGE ( 'NONE', *, *, #15968, .T. ) ;
#8268 = ORIENTED_EDGE ( 'NONE', *, *, #5792, .F. ) ;
#8269 = CARTESIAN_POINT ( 'NONE',  ( -72.50948914387967648, -26.68861478777332508, -4.330127018922180326 ) ) ;
#8270 = EDGE_CURVE ( 'NONE', #13292, #7705, #12072, .T. ) ;
#8271 = EDGE_CURVE ( 'NONE', #2601, #7195, #10385, .T. ) ;
#8272 = FACE_BOUND ( 'NONE', #5043, .T. ) ;
#8273 = ADVANCED_FACE ( 'NONE', ( #7465 ), #17536, .T. ) ;
#8274 = SURFACE_STYLE_USAGE ( .BOTH. , #784 ) ;
#8275 = VERTEX_POINT ( 'NONE', #4518 ) ;
#8276 = AXIS2_PLACEMENT_3D ( 'NONE', #5211, #18433, #10966 ) ;
#8277 = FACE_OUTER_BOUND ( 'NONE', #12038, .T. ) ;
#8278 = VERTEX_POINT ( 'NONE', #16098 ) ;
#8279 = PLANE ( 'NONE',  #2121 ) ;
#8280 = DIRECTION ( 'NONE',  ( -0.1566598588826321747, 0.9876526153536343555, 0.000000000000000000 ) ) ;
#8281 = CARTESIAN_POINT ( 'NONE',  ( 10.28861223506262412, -76.32329101363113466, 9.043241838514131834E-15 ) ) ;
#8282 = DIRECTION ( 'NONE',  ( -0.9876526153536341335, -0.1566598588826327021, 0.000000000000000000 ) ) ;
#8283 = VERTEX_POINT ( 'NONE', #1959 ) ;
#8284 = CARTESIAN_POINT ( 'NONE',  ( -62.00000000000000000, 0.000000000000000000, 20.00000000000001776 ) ) ;
#8285 = DIRECTION ( 'NONE',  ( -0.1566598588826321192, 0.9876526153536342445, 7.798540720466730171E-17 ) ) ;
#8286 = VERTEX_POINT ( 'NONE', #3174 ) ;
#8287 = VERTEX_POINT ( 'NONE', #13497 ) ;
#8288 = CARTESIAN_POINT ( 'NONE',  ( -3.538524379888208227, -78.51652903798800764, 21.65063509461100821 ) ) ;
#8289 = CIRCLE ( 'NONE', #110, 1.499999999999999556 ) ;
#8290 = VERTEX_POINT ( 'NONE', #1771 ) ;
#8291 = LINE ( 'NONE', #16743, #11522 ) ;
#8292 = EDGE_CURVE ( 'NONE', #18427, #4539, #7784, .T. ) ;
#8293 = CARTESIAN_POINT ( 'NONE',  ( -54.89646037827696290, -86.66284169988485075, 12.99038105676661203 ) ) ;
#8294 = ORIENTED_EDGE ( 'NONE', *, *, #16256, .F. ) ;
#8295 = EDGE_CURVE ( 'NONE', #11597, #11722, #2927, .T. ) ;
#8296 = EDGE_CURVE ( 'NONE', #8123, #1233, #11885, .T. ) ;
#8297 = CARTESIAN_POINT ( 'NONE',  ( -70.47070042840788062, 45.20028515864974850, 5.277796196381517646 ) ) ;
#8298 = DIRECTION ( 'NONE',  ( 0.000000000000000000, 0.000000000000000000, 1.000000000000000000 ) ) ;
#8299 = CARTESIAN_POINT ( 'NONE',  ( 3.231158466157554976, 19.73726462726228092, -24.99999999999998934 ) ) ;
#8300 = CARTESIAN_POINT ( 'NONE',  ( -12.92122422574768592, -80.00479769737299307, 1.443110928631665584E-14 ) ) ;
#8301 = EDGE_LOOP ( 'NONE', ( #17859, #11855, #4162, #8528 ) ) ;
#8302 = DIRECTION ( 'NONE',  ( -0.1566598588826321192, 0.9876526153536342445, 7.798540720466730171E-17 ) ) ;
#8303 = ORIENTED_EDGE ( 'NONE', *, *, #15529, .F. ) ;
#8304 = VERTEX_POINT ( 'NONE', #2237 ) ;
#8305 = FACE_BOUND ( 'NONE', #3711, .T. ) ;
#8306 = DIRECTION ( 'NONE',  ( 0.000000000000000000, 0.000000000000000000, -1.000000000000000000 ) ) ;
#8307 = EDGE_LOOP ( 'NONE', ( #15793, #11818, #8387, #13130 ) ) ;
#8308 = ORIENTED_EDGE ( 'NONE', *, *, #6851, .T. ) ;
#8309 = DIRECTION ( 'NONE',  ( -0.000000000000000000, -0.000000000000000000, -1.000000000000000000 ) ) ;
#8310 = VERTEX_POINT ( 'NONE', #1041 ) ;
#8311 = EDGE_LOOP ( 'NONE', ( #11322, #5901 ) ) ;
#8312 = LINE ( 'NONE', #2323, #1844 ) ;
#8313 = DIRECTION ( 'NONE',  ( 0.000000000000000000, 0.000000000000000000, 1.000000000000000000 ) ) ;
#8314 = CARTESIAN_POINT ( 'NONE',  ( -128.8626752476364459, 9.172828411137484039, 4.224609204322598899 ) ) ;
#8315 = ADVANCED_FACE ( 'NONE', ( #17919 ), #13779, .F. ) ;
#8316 = DIRECTION ( 'NONE',  ( -0.9876526153536336894, -0.1566598588826349503, 0.000000000000000000 ) ) ;
#8317 = DIRECTION ( 'NONE',  ( -0.9876526153536341335, -0.1566598588826327021, 0.000000000000000000 ) ) ;
#8318 =( LENGTH_UNIT ( ) NAMED_UNIT ( * ) SI_UNIT ( .MILLI., .METRE. ) );
#8319 = FACE_OUTER_BOUND ( 'NONE', #10266, .T. ) ;
#8320 = EDGE_LOOP ( 'NONE', ( #2845, #6481, #15057, #1163 ) ) ;
#8321 = DIRECTION ( 'NONE',  ( 0.000000000000000000, 0.000000000000000000, 1.000000000000000000 ) ) ;
#8322 = EDGE_CURVE ( 'NONE', #6756, #17136, #16886, .T. ) ;
#8323 = DIRECTION ( 'NONE',  ( 0.000000000000000000, 0.000000000000000000, -1.000000000000000000 ) ) ;
#8324 = CARTESIAN_POINT ( 'NONE',  ( -84.16800061185418258, 32.38614985672617763, 35.00001200000001234 ) ) ;
#8325 = DIRECTION ( 'NONE',  ( -0.1566598588826321192, 0.9876526153536342445, 7.798540720466731404E-17 ) ) ;
#8327 = VERTEX_POINT ( 'NONE', #18213 ) ;
#8326 = DIRECTION ( 'NONE',  ( -0.1566598588826321747, 0.9876526153536343555, 0.000000000000000000 ) ) ;
#8328 = CARTESIAN_POINT ( 'NONE',  ( -90.00000000000000000, 34.99999999999999289, -30.00000000000000355 ) ) ;
#8329 = AXIS2_PLACEMENT_3D ( 'NONE', #17677, #6279, #399 ) ;
#8330 = DIRECTION ( 'NONE',  ( 1.000000000000000000, 0.000000000000000000, -0.000000000000000000 ) ) ;
#8331 = ORIENTED_EDGE ( 'NONE', *, *, #16368, .F. ) ;
#8332 = ORIENTED_EDGE ( 'NONE', *, *, #9224, .F. ) ;
#8333 = VERTEX_POINT ( 'NONE', #8017 ) ;
#8334 = CARTESIAN_POINT ( 'NONE',  ( -32.67427653282028643, -83.13799487502562613, -17.32050807568878525 ) ) ;
#8335 = ORIENTED_EDGE ( 'NONE', *, *, #16291, .T. ) ;
#8336 = CARTESIAN_POINT ( 'NONE',  ( -66.08974714408108753, -25.67032570503621258, -21.65063509461097979 ) ) ;
#8337 = CARTESIAN_POINT ( 'NONE',  ( -42.87991068327077926, -21.98881902129438259, 12.99038105676661736 ) ) ;
#8338 = EDGE_LOOP ( 'NONE', ( #5724, #3369, #12215, #17806 ) ) ;
#8339 = CARTESIAN_POINT ( 'NONE',  ( -6.995308533625909320, -79.06483854407721878, 12.99038105676660848 ) ) ;
#8340 = DIRECTION ( 'NONE',  ( 0.1856185419698755945, -0.9826218788918641422, 0.000000000000000000 ) ) ;
#8341 = EDGE_CURVE ( 'NONE', #16044, #15425, #14140, .T. ) ;
#8342 = EDGE_CURVE ( 'NONE', #4043, #7702, #11390, .T. ) ;
#8343 = DIRECTION ( 'NONE',  ( -0.1566598588826321747, 0.9876526153536343555, 0.000000000000000000 ) ) ;
#8344 = AXIS2_PLACEMENT_3D ( 'NONE', #10933, #6992, #16940 ) ;
#8345 = DIRECTION ( 'NONE',  ( 0.000000000000000000, 0.000000000000000000, 1.000000000000000000 ) ) ;
#8346 = EDGE_CURVE ( 'NONE', #16242, #1233, #10485, .T. ) ;
#8347 = DIRECTION ( 'NONE',  ( -0.000000000000000000, -0.000000000000000000, -1.000000000000000000 ) ) ;
#8348 = VERTEX_POINT ( 'NONE', #11032 ) ;
#8349 = VERTEX_POINT ( 'NONE', #10672 ) ;
#8350 = CARTESIAN_POINT ( 'NONE',  ( -13.25033222266188915, -17.28902325481541880, -21.65063509461098334 ) ) ;
#8351 = VECTOR ( 'NONE', #4395, 1000.000000000000000 ) ;
#8352 = FACE_BOUND ( 'NONE', #9553, .T. ) ;
#8353 = ADVANCED_FACE ( 'NONE', ( #6521 ), #5067, .F. ) ;
#8354 = DIRECTION ( 'NONE',  ( -0.1566598588826321192, 0.9876526153536342445, 7.798540720466730171E-17 ) ) ;
#8355 = EDGE_CURVE ( 'NONE', #15832, #5613, #13603, .T. ) ;
#8356 = EDGE_CURVE ( 'NONE', #405, #16739, #18727, .T. ) ;
#8357 = AXIS2_PLACEMENT_3D ( 'NONE', #3764, #5220, #9569 ) ;
#8358 = ORIENTED_EDGE ( 'NONE', *, *, #7026, .T. ) ;
#8359 = FACE_OUTER_BOUND ( 'NONE', #10029, .T. ) ;
#8360 = CARTESIAN_POINT ( 'NONE',  ( -70.20507591625822386, -89.09106951256563889, -17.32050807568878525 ) ) ;
#8361 = VECTOR ( 'NONE', #3765, 1000.000000000000000 ) ;
#8362 = CYLINDRICAL_SURFACE ( 'NONE', #14234, 1.500000000000001554 ) ;
#8363 = DIRECTION ( 'NONE',  ( 0.000000000000000000, 0.000000000000000000, 1.000000000000000000 ) ) ;
#8364 = VERTEX_POINT ( 'NONE', #12473 ) ;
#8365 = B_SPLINE_CURVE_WITH_KNOTS ( 'NONE', 3,
 ( #4567, #6099, #496, #11843 ),
 .UNSPECIFIED., .F., .F.,
 ( 4, 4 ),
 ( 0.000000000000000000, 0.003000475340473865958 ),
 .UNSPECIFIED. ) ;
#8366 = DIRECTION ( 'NONE',  ( -0.1566598588826321192, 0.9876526153536342445, 7.798540720466731404E-17 ) ) ;
#8367 = ORIENTED_EDGE ( 'NONE', *, *, #15094, .F. ) ;
#8368 = VERTEX_POINT ( 'NONE', #10841 ) ;
#8369 = ORIENTED_EDGE ( 'NONE', *, *, #2582, .F. ) ;
#8370 = DIRECTION ( 'NONE',  ( -0.1566598588826321747, 0.9876526153536343555, 0.000000000000000000 ) ) ;
#8371 = AXIS2_PLACEMENT_3D ( 'NONE', #15260, #882, #3497 ) ;
#8372 = ORIENTED_EDGE ( 'NONE', *, *, #14376, .F. ) ;
#8373 = FACE_OUTER_BOUND ( 'NONE', #13560, .T. ) ;
#8374 = CARTESIAN_POINT ( 'NONE',  ( -79.13358446461874962, -32.80182680616118773, 17.32050807568881723 ) ) ;
#8375 = VECTOR ( 'NONE', #4119, 1000.000000000000000 ) ;
#8376 = CARTESIAN_POINT ( 'NONE',  ( 1.893565004556770903, -77.65489981413351472, 17.32050807568880657 ) ) ;
#8377 = ITEM_DEFINED_TRANSFORMATION ( 'NONE', 'NONE', #8985,  #18772 ) ;
#8378 = CARTESIAN_POINT ( 'NONE',  ( -61.31620237807555895, -87.68113078262196325, 21.65063509461101532 ) ) ;
#8379 = AXIS2_PLACEMENT_3D ( 'NONE', #15002, #2018, #423 ) ;
#8380 = CARTESIAN_POINT ( 'NONE',  ( -129.1404785418517918, -2.850701963179328668, 5.500000000000000000 ) ) ;
#8381 = DIRECTION ( 'NONE',  ( -1.000000000000000000, 0.000000000000000000, -3.208277787129350839E-17 ) ) ;
#8382 = EDGE_CURVE ( 'NONE', #1532, #14684, #3819, .T. ) ;
#8383 = FACE_OUTER_BOUND ( 'NONE', #351, .T. ) ;
#8384 = DIRECTION ( 'NONE',  ( 0.000000000000000000, 0.000000000000000000, 1.000000000000000000 ) ) ;
#8385 = ORIENTED_EDGE ( 'NONE', *, *, #3380, .T. ) ;
#8386 = EDGE_CURVE ( 'NONE', #2695, #15443, #4218, .T. ) ;
#8387 = ORIENTED_EDGE ( 'NONE', *, *, #219, .T. ) ;
#8388 = FACE_OUTER_BOUND ( 'NONE', #1261, .T. ) ;
#8389 = CARTESIAN_POINT ( 'NONE',  ( -50.28730529842301422, -23.16376796291411466, 1.908195823574487804E-14 ) ) ;
#8390 = ORIENTED_EDGE ( 'NONE', *, *, #12216, .T. ) ;
#8391 = AXIS2_PLACEMENT_3D ( 'NONE', #4983, #7952, #15049 ) ;
#8392 = ADVANCED_FACE ( 'NONE', ( #15219 ), #16772, .F. ) ;
#8393 = CYLINDRICAL_SURFACE ( 'NONE', #9994, 1.500000000000001554 ) ;
#8394 = AXIS2_PLACEMENT_3D ( 'NONE', #6339, #3002, #4790 ) ;
#8395 = ORIENTED_EDGE ( 'NONE', *, *, #5322, .T. ) ;
#8396 = CARTESIAN_POINT ( 'NONE',  ( -105.1664215174088355, -37.48287248576487940, 2.500000000000000000 ) ) ;
#8397 = AXIS2_PLACEMENT_3D ( 'NONE', #17151, #9758, #2541 ) ;
#8398 = CARTESIAN_POINT ( 'NONE',  ( -61.15148406731292852, -24.88702641062307208, 21.65063509461102242 ) ) ;
#8399 = VERTEX_POINT ( 'NONE', #8117 ) ;
#8400 = DIRECTION ( 'NONE',  ( -0.1566598588826321747, 0.9876526153536343555, 0.000000000000000000 ) ) ;
#8401 = CARTESIAN_POINT ( 'NONE',  ( -8.516422466834198346, -21.60064689605303911, -8.660254037844380193 ) ) ;
#8402 = PRESENTATION_LAYER_ASSIGNMENT (  '', '', ( #9605 ) ) ;
#8403 = CARTESIAN_POINT ( 'NONE',  ( -9.464440072009985272, -79.45648819128378193, 1.424741226644455312E-14 ) ) ;
#8404 = SURFACE_STYLE_USAGE ( .BOTH. , #15883 ) ;
#8405 = CIRCLE ( 'NONE', #13519, 1.499999999999999556 ) ;
#8406 = DIRECTION ( 'NONE',  ( -0.9876526153536336894, -0.1566598588826350336, 0.000000000000000000 ) ) ;
#8407 = EDGE_LOOP ( 'NONE', ( #16320, #6668 ) ) ;
#8408 = DIRECTION ( 'NONE',  ( 0.000000000000000000, 0.000000000000000000, 1.000000000000000000 ) ) ;
#8409 = DIRECTION ( 'NONE',  ( -0.1566598588826321747, 0.9876526153536343555, 0.000000000000000000 ) ) ;
#8410 = DIRECTION ( 'NONE',  ( -1.000000000000000000, 0.000000000000000000, 0.000000000000000000 ) ) ;
#8411 = ORIENTED_EDGE ( 'NONE', *, *, #10984, .F. ) ;
#8412 = LINE ( 'NONE', #12764, #18212 ) ;
#8413 = CARTESIAN_POINT ( 'NONE',  ( -77.11859967870812227, -1.071530569176025516, 6.007857748507488438 ) ) ;
#8415 = VERTEX_POINT ( 'NONE', #9343 ) ;
#8414 = CARTESIAN_POINT ( 'NONE',  ( -60.16383145195931803, -24.73036655174042764, -8.660254037844380193 ) ) ;
#8416 = ADVANCED_FACE ( 'NONE', ( #15411 ), #2435, .F. ) ;
#8417 = CARTESIAN_POINT ( 'NONE',  ( -20.32861884089991023, -81.17974663899273935, 21.65063509461101532 ) ) ;
#8418 = ORIENTED_EDGE ( 'NONE', *, *, #5996, .T. ) ;
#8419 = ORIENTED_EDGE ( 'NONE', *, *, #7149, .F. ) ;
#8420 = CIRCLE ( 'NONE', #2664, 15.83618137761394173 ) ;
#8421 = ORIENTED_EDGE ( 'NONE', *, *, #13028, .F. ) ;
#8422 = CYLINDRICAL_SURFACE ( 'NONE', #4877, 1.500000000000001554 ) ;
#8423 = EDGE_CURVE ( 'NONE', #6209, #3396, #16649, .T. ) ;
#8424 = ORIENTED_EDGE ( 'NONE', *, *, #6908, .F. ) ;
#8425 = DIRECTION ( 'NONE',  ( -0.1566598588826321747, 0.9876526153536343555, 0.000000000000000000 ) ) ;
#8426 = CARTESIAN_POINT ( 'NONE',  ( -31.52190560670403841, -20.18723064414410828, -12.99038105676658006 ) ) ;
#8427 = EDGE_CURVE ( 'NONE', #11472, #6385, #3298, .T. ) ;
#8428 = AXIS2_PLACEMENT_3D ( 'NONE', #9419, #12523, #12324 ) ;
#8429 = EDGE_LOOP ( 'NONE', ( #14092, #4746, #3986, #9955 ) ) ;
#8430 = FACE_OUTER_BOUND ( 'NONE', #3753, .T. ) ;
#8431 = CYLINDRICAL_SURFACE ( 'NONE', #16907, 1.500000000000001554 ) ;
#8432 = AXIS2_PLACEMENT_3D ( 'NONE', #810, #11209, #6592 ) ;
#8433 = AXIS2_PLACEMENT_3D ( 'NONE', #9623, #8490, #2513 ) ;
#8434 = CARTESIAN_POINT ( 'NONE',  ( 2.881217619910392269, -77.49823995525089515, 12.99038105676660493 ) ) ;
#8435 = DIRECTION ( 'NONE',  ( -0.9876526153536341335, -0.1566598588826327021, 0.000000000000000000 ) ) ;
#8436 = CARTESIAN_POINT ( 'NONE',  ( -66.25446545484369665, -88.46443007703510375, -21.65063509461098690 ) ) ;
#8437 = ORIENTED_EDGE ( 'NONE', *, *, #13564, .T. ) ;
#8438 = CARTESIAN_POINT ( 'NONE',  ( -309.1404785418517918, -2.850701963179328668, 9.951701414186818625E-16 ) ) ;
#8439 = CARTESIAN_POINT ( 'NONE',  ( -42.87991068327077926, -21.98881902129438615, 21.65063509461101887 ) ) ;
#8440 = DIRECTION ( 'NONE',  ( 0.000000000000000000, 0.000000000000000000, 1.000000000000000000 ) ) ;
#8441 = EDGE_LOOP ( 'NONE', ( #11840, #1120, #6191, #3114 ) ) ;
#8442 = EDGE_CURVE ( 'NONE', #15648, #12551, #16561, .T. ) ;
#8443 = CLOSED_SHELL ( 'NONE', ( #2586, #1397, #7974, #16024, #1015, #5693, #10181, #5429, #13190, #14541 ) ) ;
#8444 = DIRECTION ( 'NONE',  ( -0.9876526153536341335, -0.1566598588826327021, 0.000000000000000000 ) ) ;
#8445 = ADVANCED_FACE ( 'NONE', ( #5761 ), #16147, .F. ) ;
#8446 = CIRCLE ( 'NONE', #18778, 1.500000000000000000 ) ;
#8447 = VERTEX_POINT ( 'NONE', #3139 ) ;
#8448 = ORIENTED_EDGE ( 'NONE', *, *, #18655, .T. ) ;
#8449 = CARTESIAN_POINT ( 'NONE',  ( -66.29410046502155751, -30.76524864068697696, 8.660254037844417496 ) ) ;
#8450 = CIRCLE ( 'NONE', #4195, 1.500000000000000888 ) ;
#8451 = AXIS2_PLACEMENT_3D ( 'NONE', #13288, #323, #16337 ) ;
#8452 = FACE_BOUND ( 'NONE', #18668, .T. ) ;
#8453 = EDGE_CURVE ( 'NONE', #5884, #14364, #8474, .T. ) ;
#8454 = CARTESIAN_POINT ( 'NONE',  ( -176.1167811578620501, -139.6880237571007513, -2.500000000000000000 ) ) ;
#8455 = AXIS2_PLACEMENT_3D ( 'NONE', #9499, #15266, #6673 ) ;
#8456 = VECTOR ( 'NONE', #14324, 1000.000000000000000 ) ;
#8457 = LINE ( 'NONE', #1274, #17556 ) ;
#8458 = AXIS2_PLACEMENT_3D ( 'NONE', #8876, #14562, #10099 ) ;
#8459 = CARTESIAN_POINT ( 'NONE',  ( 11.59211860341529210, 6.314490184041242848, -20.00000000000000355 ) ) ;
#8460 = DIRECTION ( 'NONE',  ( -0.1566598588826321192, 0.9876526153536342445, 7.798540720466730171E-17 ) ) ;
#8461 = AXIS2_PLACEMENT_3D ( 'NONE', #1666, #10005, #5932 ) ;
#8462 = AXIS2_PLACEMENT_3D ( 'NONE', #1433, #12966, #7 ) ;
#8463 = AXIS2_PLACEMENT_3D ( 'NONE', #4323, #17242, #4221 ) ;
#8465 = EDGE_CURVE ( 'NONE', #14662, #10352, #9973, .T. ) ;
#8464 = CARTESIAN_POINT ( 'NONE',  ( -52.96079015774754595, -28.65034054577145994, 17.32050807568881723 ) ) ;
#8466 = DIRECTION ( 'NONE',  ( -0.1566598588826321747, 0.9876526153536343555, 0.000000000000000000 ) ) ;
#8468 = ORIENTED_EDGE ( 'NONE', *, *, #5749, .F. ) ;
#8467 = EDGE_CURVE ( 'NONE', #1369, #12170, #14816, .T. ) ;
#8469 = VERTEX_POINT ( 'NONE', #11503 ) ;
#8470 = AXIS2_PLACEMENT_3D ( 'NONE', #15947, #9978, #5633 ) ;
#8471 = ORIENTED_EDGE ( 'NONE', *, *, #12545, .T. ) ;
#8472 = CARTESIAN_POINT ( 'NONE',  ( 9.300959619709004755, -76.47995087251376845, -12.99038105676658894 ) ) ;
#8473 = EDGE_CURVE ( 'NONE', #10566, #3641, #15687, .T. ) ;
#8474 = CIRCLE ( 'NONE', #13906, 1.500000000000000888 ) ;
#8475 = EDGE_CURVE ( 'NONE', #3563, #3927, #6665, .T. ) ;
#8476 = ORIENTED_EDGE ( 'NONE', *, *, #2168, .T. ) ;
#8477 = CIRCLE ( 'NONE', #8771, 1.500000000000000444 ) ;
#8478 = VERTEX_POINT ( 'NONE', #1313 ) ;
#8479 = CARTESIAN_POINT ( 'NONE',  ( -2.057045456857756971, -78.28153924966404986, 4.330127018922209636 ) ) ;
#8480 = DIRECTION ( 'NONE',  ( -0.9876526153536336894, -0.1566598588826349503, 0.000000000000000000 ) ) ;
#8481 = CIRCLE ( 'NONE', #12680, 2.200000000000000178 ) ;
#8482 = EDGE_LOOP ( 'NONE', ( #2980, #3115, #11059, #8013 ) ) ;
#8483 = VECTOR ( 'NONE', #6786, 1000.000000000000000 ) ;
#8484 = DIRECTION ( 'NONE',  ( -0.1566598588826321192, 0.9876526153536342445, 7.798540720466731404E-17 ) ) ;
#8485 = DIRECTION ( 'NONE',  ( 0.000000000000000000, 0.000000000000000000, 1.000000000000000000 ) ) ;
#8486 = CIRCLE ( 'NONE', #1238, 2.200000000000000622 ) ;
#8487 = DIRECTION ( 'NONE',  ( 0.000000000000000000, 0.000000000000000000, 1.000000000000000000 ) ) ;
#8489 = CARTESIAN_POINT ( 'NONE',  ( -53.90880776292333820, -86.50618184100221697, 1.424741226644455312E-14 ) ) ;
#8488 = VECTOR ( 'NONE', #14524, 1000.000000000000000 ) ;
#8490 = DIRECTION ( 'NONE',  ( -0.1566598588826321747, 0.9876526153536343555, 0.000000000000000000 ) ) ;
#8491 = FACE_OUTER_BOUND ( 'NONE', #4080, .T. ) ;
#8492 = ORIENTED_EDGE ( 'NONE', *, *, #5114, .T. ) ;
#8493 = ORIENTED_EDGE ( 'NONE', *, *, #5812, .T. ) ;
#8494 = DIRECTION ( 'NONE',  ( -0.1566598588826321192, 0.9876526153536342445, 7.798540720466731404E-17 ) ) ;
#8495 = FACE_BOUND ( 'NONE', #9874, .T. ) ;
#8496 = AXIS2_PLACEMENT_3D ( 'NONE', #5948, #17642, #17438 ) ;
#8497 = DIRECTION ( 'NONE',  ( 8.693966348389027220E-17, -1.991237296706374949E-16, 1.000000000000000000 ) ) ;
#8498 = VERTEX_POINT ( 'NONE', #8932 ) ;
#8499 = DIRECTION ( 'NONE',  ( -0.1566598588826321192, 0.9876526153536342445, 7.798540720466731404E-17 ) ) ;
#8500 = ORIENTED_EDGE ( 'NONE', *, *, #10970, .T. ) ;
#8501 = AXIS2_PLACEMENT_3D ( 'NONE', #2701, #8494, #14277 ) ;
#8502 = DIRECTION ( 'NONE',  ( -0.1566598588826321192, 0.9876526153536342445, 7.798540720466731404E-17 ) ) ;
#8503 = EDGE_CURVE ( 'NONE', #1233, #16242, #11474, .T. ) ;
#8504 = ORIENTED_EDGE ( 'NONE', *, *, #9567, .F. ) ;
#8505 = CARTESIAN_POINT ( 'NONE',  ( -127.6870874808773380, 9.532027616443281559, 2.921574671186279559 ) ) ;
#8506 = EDGE_CURVE ( 'NONE', #5893, #13704, #17609, .T. ) ;
#8507 = DIRECTION ( 'NONE',  ( -0.1566598588826321747, 0.9876526153536343555, 0.000000000000000000 ) ) ;
#8508 = AXIS2_PLACEMENT_3D ( 'NONE', #8185, #13954, #5338 ) ;
#8509 = CARTESIAN_POINT ( 'NONE',  ( -62.63296299034339398, -25.12201619894700499, -12.99038105676658006 ) ) ;
#8510 = CARTESIAN_POINT ( 'NONE',  ( -7.528769851480577202, -21.44398703717040888, -12.99038105676658006 ) ) ;
#8511 = CONICAL_SURFACE ( 'NONE', #14258, 12.74754878398196567, 0.01745329251994333364 ) ;
#8512 = FILL_AREA_STYLE_COLOUR ( '', #16896 ) ;
#8513 = EDGE_LOOP ( 'NONE', ( #11635, #2840, #2788, #15265 ) ) ;
#8514 = DIRECTION ( 'NONE',  ( -0.1566598588826321192, 0.9876526153536342445, 7.798540720466730171E-17 ) ) ;
#8515 = FACE_OUTER_BOUND ( 'NONE', #4572, .T. ) ;
#8516 = AXIS2_PLACEMENT_3D ( 'NONE', #17708, #4678, #3249 ) ;
#8517 = LINE ( 'NONE', #6652, #1082 ) ;
#8518 = CARTESIAN_POINT ( 'NONE',  ( -9.299721761247353058, -16.66238381928489787, 8.660254037844413944 ) ) ;
#8519 = ORIENTED_EDGE ( 'NONE', *, *, #16833, .F. ) ;
#8520 = DIRECTION ( 'NONE',  ( 0.000000000000000000, 0.000000000000000000, 1.000000000000000000 ) ) ;
#8521 = AXIS2_PLACEMENT_3D ( 'NONE', #17043, #10834, #13980 ) ;
#8523 = ORIENTED_EDGE ( 'NONE', *, *, #11659, .T. ) ;
#8522 = CARTESIAN_POINT ( 'NONE',  ( -15.22563745336913144, -17.60234297258069347, 4.330127018922218518 ) ) ;
#8524 = CIRCLE ( 'NONE', #17934, 12.83663829214476060 ) ;
#8525 = DIRECTION ( 'NONE',  ( -0.1566598588826321192, 0.9876526153536342445, 7.798540720466730171E-17 ) ) ;
#8526 = CARTESIAN_POINT ( 'NONE',  ( -46.33669483700847280, -22.53712852738359729, 21.65063509461102242 ) ) ;
#8527 = VERTEX_POINT ( 'NONE', #15589 ) ;
#8528 = ORIENTED_EDGE ( 'NONE', *, *, #17143, .T. ) ;
#8529 = DIRECTION ( 'NONE',  ( -1.000000000000000000, 0.000000000000000000, 0.000000000000000000 ) ) ;
#8530 = EDGE_CURVE ( 'NONE', #8287, #4436, #2812, .T. ) ;
#8531 = VECTOR ( 'NONE', #15899, 1000.000000000000000 ) ;
#8532 = VERTEX_POINT ( 'NONE', #5373 ) ;
#8533 = CIRCLE ( 'NONE', #3345, 20.00000000000001066 ) ;
#8534 = CARTESIAN_POINT ( 'NONE',  ( -48.02252708097940825, -27.86704125135829813, -8.660254037844380193 ) ) ;
#8535 = DIRECTION ( 'NONE',  ( 1.000000000000000000, 0.000000000000000000, 0.000000000000000000 ) ) ;
#8536 = DIRECTION ( 'NONE',  ( -0.1566598588826321192, 0.9876526153536342445, 7.798540720466731404E-17 ) ) ;
#8537 = CARTESIAN_POINT ( 'NONE',  ( -69.54653129781877396, -26.21863521112544504, 21.65063509461101887 ) ) ;
#8538 = VECTOR ( 'NONE', #11530, 1000.000000000000000 ) ;
#8539 = EDGE_CURVE ( 'NONE', #10405, #11588, #4571, .T. ) ;
#8540 = CARTESIAN_POINT ( 'NONE',  ( -70.00000000000000000, 44.99999999999999289, -25.00000000000000000 ) ) ;
#8541 = ORIENTED_EDGE ( 'NONE', *, *, #15274, .F. ) ;
#8542 = DIRECTION ( 'NONE',  ( -0.9876526153536336894, -0.1566598588826349503, 0.000000000000000000 ) ) ;
#8543 = FACE_BOUND ( 'NONE', #16828, .T. ) ;
#8544 = EDGE_LOOP ( 'NONE', ( #15353, #6649, #6585, #5151, #17544, #4176, #10727, #953 ) ) ;
#8545 = DIRECTION ( 'NONE',  ( -0.1566598588826321192, 0.9876526153536342445, 7.798540720466731404E-17 ) ) ;
#8546 = ORIENTED_EDGE ( 'NONE', *, *, #2134, .F. ) ;
#8547 = VECTOR ( 'NONE', #16054, 1000.000000000000000 ) ;
#8548 = ORIENTED_EDGE ( 'NONE', *, *, #17546, .F. ) ;
#8549 = CYLINDRICAL_SURFACE ( 'NONE', #17568, 1.500000000000001554 ) ;
#8550 = VERTEX_POINT ( 'NONE', #10348 ) ;
#8551 = EDGE_LOOP ( 'NONE', ( #16604, #13987 ) ) ;
#8552 = DIRECTION ( 'NONE',  ( -0.1566598588826321192, 0.9876526153536342445, 7.798540720466731404E-17 ) ) ;
#8553 = CIRCLE ( 'NONE', #996, 1.500000000000001332 ) ;
#8554 = CARTESIAN_POINT ( 'NONE',  ( -35.47251606811855851, -20.81387007967463632, -8.660254037844380193 ) ) ;
#8555 = CIRCLE ( 'NONE', #375, 1.499999999999999556 ) ;
#8556 = CARTESIAN_POINT ( 'NONE',  ( -77.24748271550588186, -0.7169195224846902637, -5.646145272226924305 ) ) ;
#8557 = CIRCLE ( 'NONE', #14883, 1.500000000000001332 ) ;
#8558 = ADVANCED_FACE ( 'NONE', ( #6902 ), #14372, .F. ) ;
#8559 = CARTESIAN_POINT ( 'NONE',  ( -2.200000000000000178, 0.000000000000000000, 25.00000000000000000 ) ) ;
#8560 = ORIENTED_EDGE ( 'NONE', *, *, #11008, .T. ) ;
#8561 = ORIENTED_EDGE ( 'NONE', *, *, #7682, .F. ) ;
#8562 = AXIS2_PLACEMENT_3D ( 'NONE', #312, #3500, #13459 ) ;
#8563 = FACE_OUTER_BOUND ( 'NONE', #849, .T. ) ;
#8564 = DIRECTION ( 'NONE',  ( -0.1566598588826321192, 0.9876526153536342445, 7.798540720466730171E-17 ) ) ;
#8566 = ADVANCED_FACE ( 'NONE', ( #9821 ), #8511, .T. ) ;
#8565 = DIRECTION ( 'NONE',  ( -0.9876526153536336894, -0.1566598588826350336, 0.000000000000000000 ) ) ;
#8567 = VERTEX_POINT ( 'NONE', #2613 ) ;
#8568 = CARTESIAN_POINT ( 'NONE',  ( -70.24471092643608472, -31.39188807621751209, -21.65063509461098334 ) ) ;
#8569 = EDGE_CURVE ( 'NONE', #15025, #2420, #7893, .T. ) ;
#8570 = ORIENTED_EDGE ( 'NONE', *, *, #3353, .T. ) ;
#8571 = ORIENTED_EDGE ( 'NONE', *, *, #3852, .T. ) ;
#8572 = ORIENTED_EDGE ( 'NONE', *, *, #6488, .T. ) ;
#8573 = DIRECTION ( 'NONE',  ( -0.1566598588826321192, 0.9876526153536342445, 7.798540720466731404E-17 ) ) ;
#8574 = ORIENTED_EDGE ( 'NONE', *, *, #4849, .F. ) ;
#8575 = VERTEX_POINT ( 'NONE', #18599 ) ;
#8576 = FACE_BOUND ( 'NONE', #7652, .T. ) ;
#8577 = CARTESIAN_POINT ( 'NONE',  ( -16.87183468716221313, -80.63143713290354242, 12.99038105676661203 ) ) ;
#8578 = ORIENTED_EDGE ( 'NONE', *, *, #8066, .T. ) ;
#8579 = CIRCLE ( 'NONE', #398, 1.500000000000000000 ) ;
#8580 = CARTESIAN_POINT ( 'NONE',  ( -49.95819730150879678, -85.87954240547168183, 21.65063509461101532 ) ) ;
#8581 = CARTESIAN_POINT ( 'NONE',  ( -71.72618984946653597, -31.62687786454144856, 4.330127018922217630 ) ) ;
#8582 = DIRECTION ( 'NONE',  ( -0.1566598588826321192, 0.9876526153536342445, 7.798540720466730171E-17 ) ) ;
#8583 = EDGE_LOOP ( 'NONE', ( #6870, #7019 ) ) ;
#8584 = EDGE_CURVE ( 'NONE', #9621, #17370, #5566, .T. ) ;
#8585 = EDGE_CURVE ( 'NONE', #14458, #4359, #17239, .T. ) ;
#8586 = DIRECTION ( 'NONE',  ( -0.1566598588826321192, 0.9876526153536342445, 7.798540720466730171E-17 ) ) ;
#8587 = EDGE_CURVE ( 'NONE', #4058, #16216, #4554, .T. ) ;
#8588 = CARTESIAN_POINT ( 'NONE',  ( -72.50948914387967648, -26.68861478777332152, -12.99038105676658006 ) ) ;
#8589 = ORIENTED_EDGE ( 'NONE', *, *, #4950, .T. ) ;
#8590 = ORIENTED_EDGE ( 'NONE', *, *, #16052, .T. ) ;
#8591 = AXIS2_PLACEMENT_3D ( 'NONE', #15717, #2742, #8535 ) ;
#8592 = CARTESIAN_POINT ( 'NONE',  ( -85.86167379012967160, 34.32252072304513746, -35.00000000000000000 ) ) ;
#8593 = DIRECTION ( 'NONE',  ( -0.1566598588826321192, 0.9876526153536342445, 7.798540720466730171E-17 ) ) ;
#8594 = CARTESIAN_POINT ( 'NONE',  ( -309.1404785418517918, -2.850701963179328668, 9.951701414186818625E-16 ) ) ;
#8595 = CARTESIAN_POINT ( 'NONE',  ( -76.66445292623467367, -32.41017715895461038, 21.65063509461101887 ) ) ;
#8596 = VERTEX_POINT ( 'NONE', #18771 ) ;
#8597 = EDGE_LOOP ( 'NONE', ( #2340, #108 ) ) ;
#8598 = CARTESIAN_POINT ( 'NONE',  ( -53.74408945216070776, -23.71207746900332580, 1.908195823574487804E-14 ) ) ;
#8599 = DIRECTION ( 'NONE',  ( -0.1566598588826321192, 0.9876526153536342445, 7.798540720466731404E-17 ) ) ;
#8600 = CARTESIAN_POINT ( 'NONE',  ( -60.36818477289978091, -29.82528948739120267, 4.330127018922217630 ) ) ;
#8601 = CARTESIAN_POINT ( 'NONE',  ( -129.0032285637105076, 9.043624184701180013, 4.582591203971080773 ) ) ;
#8602 = AXIS2_PLACEMENT_3D ( 'NONE', #5282, #3828, #8221 ) ;
#8603 = DIRECTION ( 'NONE',  ( 0.9201637183752250371, -0.3915338189555017667, 3.511704013281690619E-17 ) ) ;
#8604 = DIRECTION ( 'NONE',  ( -0.1566598588826321192, 0.9876526153536342445, 7.798540720466731404E-17 ) ) ;
#8605 = VERTEX_POINT ( 'NONE', #6480 ) ;
#8606 = EDGE_CURVE ( 'NONE', #12283, #8278, #13277, .T. ) ;
#8607 = LINE ( 'NONE', #4227, #5424 ) ;
#8608 = EDGE_LOOP ( 'NONE', ( #14117, #770 ) ) ;
#8609 = DIRECTION ( 'NONE',  ( -0.1566598588826321192, 0.9876526153536342445, 7.798540720466731404E-17 ) ) ;
#8610 = DIRECTION ( 'NONE',  ( -0.9876526153536344665, -0.1566598588826304539, 0.000000000000000000 ) ) ;
#8611 = CARTESIAN_POINT ( 'NONE',  ( -76.17062661855784711, -32.33184722951329348, 17.32050807568881723 ) ) ;
#8612 = VERTEX_POINT ( 'NONE', #9404 ) ;
#8613 = ADVANCED_FACE ( 'NONE', ( #7514 ), #3414, .F. ) ;
#8614 = DIRECTION ( 'NONE',  ( 0.000000000000000000, 0.000000000000000000, 1.000000000000000000 ) ) ;
#8615 = ORIENTED_EDGE ( 'NONE', *, *, #2282, .T. ) ;
#8616 = DIRECTION ( 'NONE',  ( -0.1566598588826321192, 0.9876526153536342445, 7.798540720466730171E-17 ) ) ;
#8617 = EDGE_LOOP ( 'NONE', ( #16283, #5256 ) ) ;
#8618 = ORIENTED_EDGE ( 'NONE', *, *, #9241, .T. ) ;
#8619 = VERTEX_POINT ( 'NONE', #4845 ) ;
#8620 = CARTESIAN_POINT ( 'NONE',  ( -59.67000514428247016, -24.65203662229912496, 12.99038105676661736 ) ) ;
#8621 = DIRECTION ( 'NONE',  ( -0.1566598588826321747, 0.9876526153536343555, 0.000000000000000000 ) ) ;
#8622 = DIRECTION ( 'NONE',  ( 0.000000000000000000, 0.000000000000000000, 1.000000000000000000 ) ) ;
#8623 = DIRECTION ( 'NONE',  ( -0.1566598588826321192, 0.9876526153536342445, 7.798540720466730171E-17 ) ) ;
#8624 = DIRECTION ( 'NONE',  ( 1.000000000000000000, 0.000000000000000000, 0.000000000000000000 ) ) ;
#8625 = DIRECTION ( 'NONE',  ( -0.000000000000000000, -0.000000000000000000, -1.000000000000000000 ) ) ;
#8626 = DIRECTION ( 'NONE',  ( 2.671473304378624222E-16, 0.000000000000000000, 1.000000000000000000 ) ) ;
#8627 = EDGE_CURVE ( 'NONE', #8447, #11204, #4908, .T. ) ;
#8628 =( NAMED_UNIT ( * ) PLANE_ANGLE_UNIT ( ) SI_UNIT ( $, .RADIAN. ) );
#8629 = DIRECTION ( 'NONE',  ( -0.9876526153536341335, -0.1566598588826327021, 0.000000000000000000 ) ) ;
#8630 = AXIS2_PLACEMENT_3D ( 'NONE', #4832, #17762, #487 ) ;
#8631 = ORIENTED_EDGE ( 'NONE', *, *, #484, .T. ) ;
#8632 = ADVANCED_FACE ( 'NONE', ( #11850 ), #500, .F. ) ;
#8633 = EDGE_CURVE ( 'NONE', #18092, #16165, #12479, .T. ) ;
#8634 = DIRECTION ( 'NONE',  ( -0.1566598588826321747, 0.9876526153536343555, 0.000000000000000000 ) ) ;
#8635 = ORIENTED_EDGE ( 'NONE', *, *, #2540, .T. ) ;
#8636 = ORIENTED_EDGE ( 'NONE', *, *, #15257, .F. ) ;
#8637 = DIRECTION ( 'NONE',  ( -0.9876526153536336894, -0.1566598588826350336, 0.000000000000000000 ) ) ;
#8638 = EDGE_CURVE ( 'NONE', #2916, #4611, #10436, .T. ) ;
#8639 = DIRECTION ( 'NONE',  ( 1.000000000000000000, 0.000000000000000000, 0.000000000000000000 ) ) ;
#8640 = DIRECTION ( 'NONE',  ( -0.9876526153536336894, -0.1566598588826350336, 0.000000000000000000 ) ) ;
#8641 = AXIS2_PLACEMENT_3D ( 'NONE', #6327, #9237, #3358 ) ;
#8642 = LINE ( 'NONE', #17295, #13596 ) ;
#8643 = FACE_OUTER_BOUND ( 'NONE', #4542, .T. ) ;
#8644 = VERTEX_POINT ( 'NONE', #17965 ) ;
#8645 = DIRECTION ( 'NONE',  ( -0.9876526153536336894, -0.1566598588826350336, 0.000000000000000000 ) ) ;
#8646 = ORIENTED_EDGE ( 'NONE', *, *, #8931, .F. ) ;
#8647 = CARTESIAN_POINT ( 'NONE',  ( -38.92930022185625205, -21.36217958576383680, 1.214306433183764966E-14 ) ) ;
#8648 = DIRECTION ( 'NONE',  ( 0.000000000000000000, 0.000000000000000000, -1.000000000000000000 ) ) ;
#8649 = DIRECTION ( 'NONE',  ( -0.1566598588826321192, 0.9876526153536342445, 7.798540720466731404E-17 ) ) ;
#8650 = CYLINDRICAL_SURFACE ( 'NONE', #11768, 3.000000000000003109 ) ;
#8651 = MANIFOLD_SOLID_BREP ( 'Fillet1', #8443 ) ;
#8652 = DIRECTION ( 'NONE',  ( 0.000000000000000000, 0.000000000000000000, 1.000000000000000000 ) ) ;
#8653 = EDGE_LOOP ( 'NONE', ( #838, #1117, #8476, #3776 ) ) ;
#8654 = ORIENTED_EDGE ( 'NONE', *, *, #23, .T. ) ;
#8655 = ORIENTED_EDGE ( 'NONE', *, *, #18581, .T. ) ;
#8656 = CARTESIAN_POINT ( 'NONE',  ( -9.299721761247353058, -16.66238381928489787, 17.32050807568881368 ) ) ;
#8657 = ADVANCED_FACE ( 'NONE', ( #9215 ), #9300, .F. ) ;
#8658 = EDGE_LOOP ( 'NONE', ( #15874, #904 ) ) ;
#8659 = DIRECTION ( 'NONE',  ( -0.000000000000000000, -0.000000000000000000, 1.000000000000000000 ) ) ;
#8660 = CARTESIAN_POINT ( 'NONE',  ( 55.85952145814821534, 6.938893903907228378E-15, 24.99999999999998224 ) ) ;
#8661 = VECTOR ( 'NONE', #14605, 1000.000000000000000 ) ;
#8662 = EDGE_CURVE ( 'NONE', #2455, #9953, #4316, .T. ) ;
#8663 = VECTOR ( 'NONE', #13062, 1000.000000000000114 ) ;
#8664 = CARTESIAN_POINT ( 'NONE',  ( -306.1404785418517918, -2.850701963179328668, 9.951701414186818625E-16 ) ) ;
#8665 = CARTESIAN_POINT ( 'NONE',  ( -62.83731631128386397, -30.21693913459777647, 8.660254037844417496 ) ) ;
#8666 = CONTEXT_DEPENDENT_SHAPE_REPRESENTATION ( #15240, #14981 ) ;
#8667 = CARTESIAN_POINT ( 'NONE',  ( -172.0951522251743029, 56.61964399677356141, 2.500000000000000000 ) ) ;
#8668 = CARTESIAN_POINT ( 'NONE',  ( -7.818242838216901802, -16.42739403096095074, 1.579620830366336657E-14 ) ) ;
#8669 = CARTESIAN_POINT ( 'NONE',  ( -70.15512743057031742, 45.06600742248694047, -6.205119912480675737 ) ) ;
#8670 = EDGE_LOOP ( 'NONE', ( #17913, #17680, #18762, #1709 ) ) ;
#8671 = ORIENTED_EDGE ( 'NONE', *, *, #9393, .T. ) ;
#8672 = DIRECTION ( 'NONE',  ( -1.000000000000000000, 0.000000000000000000, 0.000000000000000000 ) ) ;
#8673 = CIRCLE ( 'NONE', #15316, 1.500000000000000888 ) ;
#8674 = DIRECTION ( 'NONE',  ( 0.000000000000000000, 0.000000000000000000, 1.000000000000000000 ) ) ;
#8675 = VERTEX_POINT ( 'NONE', #7616 ) ;
#8676 = EDGE_CURVE ( 'NONE', #17125, #9211, #10364, .T. ) ;
#8677 = AXIS2_PLACEMENT_3D ( 'NONE', #16479, #11805, #12183 ) ;
#8678 = VERTEX_POINT ( 'NONE', #3596 ) ;
#8679 = CARTESIAN_POINT ( 'NONE',  ( -94.14047854185179176, 6.938893903907228378E-15, 35.00000000000000000 ) ) ;
#8680 = ADVANCED_FACE ( 'NONE', ( #13379 ), #16326, .F. ) ;
#8681 = ADVANCED_FACE ( 'NONE', ( #10710 ), #16511, .F. ) ;
#8682 = DIRECTION ( 'NONE',  ( -0.1566598588826321192, 0.9876526153536342445, 7.798540720466730171E-17 ) ) ;
#8683 = CARTESIAN_POINT ( 'NONE',  ( -81.73462711737164454, 33.01666666666666572, 35.00000000000000000 ) ) ;
#8684 = CARTESIAN_POINT ( 'NONE',  ( -38.14600092744310444, -26.30044266253198160, 8.660254037844417496 ) ) ;
#8685 = CIRCLE ( 'NONE', #11682, 1.500000000000000888 ) ;
#8686 = DIRECTION ( 'NONE',  ( -0.9998476951563911586, 2.137303368083795934E-18, -0.01745240643728354635 ) ) ;
#8687 = CIRCLE ( 'NONE', #523, 1.500000000000001332 ) ;
#8688 = DIRECTION ( 'NONE',  ( -0.1566598588826321747, 0.9876526153536343555, 0.000000000000000000 ) ) ;
#8689 = DIRECTION ( 'NONE',  ( -0.000000000000000000, -0.000000000000000000, 1.000000000000000000 ) ) ;
#8690 = ORIENTED_EDGE ( 'NONE', *, *, #10923, .F. ) ;
#8691 = DIRECTION ( 'NONE',  ( -0.1566598588826321192, 0.9876526153536342445, 7.798540720466730171E-17 ) ) ;
#8692 = ORIENTED_EDGE ( 'NONE', *, *, #489, .F. ) ;
#8693 = CIRCLE ( 'NONE', #15344, 2.200000000000007283 ) ;
#8694 = DIRECTION ( 'NONE',  ( -0.9876526153536336894, -0.1566598588826349503, 0.000000000000000000 ) ) ;
#8695 = ORIENTED_EDGE ( 'NONE', *, *, #14697, .F. ) ;
#8696 = EDGE_CURVE ( 'NONE', #4036, #3838, #2485, .T. ) ;
#8697 = EDGE_CURVE ( 'NONE', #10816, #9211, #2376, .T. ) ;
#8698 = ADVANCED_FACE ( 'NONE', ( #14033 ), #18551, .F. ) ;
#8699 = CIRCLE ( 'NONE', #17801, 1.500000000000001332 ) ;
#8700 = CARTESIAN_POINT ( 'NONE',  ( -167.4745151998187680, 32.15905408292213252, 2.500000000000000000 ) ) ;
#8701 = AXIS2_PLACEMENT_3D ( 'NONE', #18172, #9420, #5146 ) ;
#8702 = CARTESIAN_POINT ( 'NONE',  ( -19.17624791478365864, -18.22898240811121440, -17.32050807568878170 ) ) ;
#8703 = EDGE_CURVE ( 'NONE', #14223, #12256, #2809, .T. ) ;
#8704 = CARTESIAN_POINT ( 'NONE',  ( -74.97862068226375243, -27.08026443497989888, -17.32050807568878170 ) ) ;
#8705 = DIRECTION ( 'NONE',  ( 0.000000000000000000, 0.000000000000000000, 1.000000000000000000 ) ) ;
#8706 = CARTESIAN_POINT ( 'NONE',  ( -35.67686938905902849, -25.90879301532540779, 12.99038105676661736 ) ) ;
#8707 = CARTESIAN_POINT ( 'NONE',  ( -17.85948730251583783, -80.78809699178616199, 8.660254037844412167 ) ) ;
#8708 = MANIFOLD_SOLID_BREP ( 'Fillet1', #6029 ) ;
#8709 = AXIS2_PLACEMENT_3D ( 'NONE', #14817, #16518, #617 ) ;
#8710 = DIRECTION ( 'NONE',  ( 0.000000000000000000, 0.000000000000000000, 1.000000000000000000 ) ) ;
#8711 = ORIENTED_EDGE ( 'NONE', *, *, #16898, .F. ) ;
#8712 = CARTESIAN_POINT ( 'NONE',  ( -5.059638313096497697, -21.05233738996382797, 1.522258424776792809E-14 ) ) ;
#8713 = CYLINDRICAL_SURFACE ( 'NONE', #14470, 1.500000000000000888 ) ;
#8714 = FACE_OUTER_BOUND ( 'NONE', #1761, .T. ) ;
#8715 = ORIENTED_EDGE ( 'NONE', *, *, #3450, .T. ) ;
#8716 = CIRCLE ( 'NONE', #12326, 1.500000000000001332 ) ;
#8717 = ORIENTED_EDGE ( 'NONE', *, *, #7777, .T. ) ;
#8718 = LINE ( 'NONE', #2562, #17559 ) ;
#8719 = VERTEX_POINT ( 'NONE', #13937 ) ;
#8720 = EDGE_LOOP ( 'NONE', ( #16017, #16788, #2918, #2929 ) ) ;
#8721 = ORIENTED_EDGE ( 'NONE', *, *, #10407, .T. ) ;
#8722 = CARTESIAN_POINT ( 'NONE',  ( -309.0881213225398483, -2.850701963179328668, -18.88854657239857815 ) ) ;
#8723 = DIRECTION ( 'NONE',  ( -0.000000000000000000, -0.000000000000000000, 1.000000000000000000 ) ) ;
#8724 = EDGE_LOOP ( 'NONE', ( #4788, #10507 ) ) ;
#8725 = DIRECTION ( 'NONE',  ( -0.1566598588826321192, 0.9876526153536342445, 7.798540720466731404E-17 ) ) ;
#8726 = VECTOR ( 'NONE', #16416, 1000.000000000000000 ) ;
#8727 = AXIS2_PLACEMENT_3D ( 'NONE', #18537, #12788, #15729 ) ;
#8728 = CARTESIAN_POINT ( 'NONE',  ( -78.35787276487999975, 0.9448187065377893212, -3.952829652586226761 ) ) ;
#8729 = EDGE_CURVE ( 'NONE', #3731, #5152, #991, .T. ) ;
#8730 = EDGE_CURVE ( 'NONE', #6631, #13791, #15824, .T. ) ;
#8731 = DIRECTION ( 'NONE',  ( 0.000000000000000000, 0.000000000000000000, 1.000000000000000000 ) ) ;
#8732 = VERTEX_POINT ( 'NONE', #12693 ) ;
#8733 = CARTESIAN_POINT ( 'NONE',  ( -40.08167114797249297, -84.31294381664535820, 12.99038105676661203 ) ) ;
#8734 = CYLINDRICAL_SURFACE ( 'NONE', #12713, 1.500000000000001554 ) ;
#8735 = CARTESIAN_POINT ( 'NONE',  ( -66.29410046502155751, -30.76524864068697696, -8.660254037844380193 ) ) ;
#8736 = DIRECTION ( 'NONE',  ( -0.1566598588826321747, 0.9876526153536343555, 0.000000000000000000 ) ) ;
#8737 = AXIS2_PLACEMENT_3D ( 'NONE', #4429, #2836, #1781 ) ;
#8738 = LINE ( 'NONE', #13093, #1197 ) ;
#8739 = VECTOR ( 'NONE', #18335, 1000.000000000000000 ) ;
#8740 = VERTEX_POINT ( 'NONE', #15263 ) ;
#8741 = ORIENTED_EDGE ( 'NONE', *, *, #17635, .F. ) ;
#8742 = ORIENTED_EDGE ( 'NONE', *, *, #596, .F. ) ;
#8743 = LINE ( 'NONE', #8472, #3348 ) ;
#8744 = ORIENTED_EDGE ( 'NONE', *, *, #18077, .T. ) ;
#8745 = DIRECTION ( 'NONE',  ( -0.9876526153536336894, -0.1566598588826350336, 0.000000000000000000 ) ) ;
#8746 = ORIENTED_EDGE ( 'NONE', *, *, #17782, .T. ) ;
#8747 = DIRECTION ( 'NONE',  ( -1.000000000000000000, 0.000000000000000000, 0.000000000000000000 ) ) ;
#8748 = AXIS2_PLACEMENT_3D ( 'NONE', #4563, #14793, #1639 ) ;
#8749 = CARTESIAN_POINT ( 'NONE',  ( -75.18297400320422241, -32.17518737063066681, -4.330127018922181215 ) ) ;
#8750 = EDGE_CURVE ( 'NONE', #14167, #12815, #5417, .T. ) ;
#8751 = CARTESIAN_POINT ( 'NONE',  ( -37.94164760650263446, -21.20551972688121367, -12.99038105676658006 ) ) ;
#8752 = CARTESIAN_POINT ( 'NONE',  ( 2.881217619910392269, -77.49823995525089515, 21.65063509461100821 ) ) ;
#8753 = DIRECTION ( 'NONE',  ( -0.000000000000000000, -0.000000000000000000, -1.000000000000000000 ) ) ;
#8754 = DIRECTION ( 'NONE',  ( 0.000000000000000000, 0.000000000000000000, 1.000000000000000000 ) ) ;
#8755 = AXIS2_PLACEMENT_3D ( 'NONE', #11478, #17314, #11203 ) ;
#8756 = CARTESIAN_POINT ( 'NONE',  ( -89.99999999999998579, -35.00000000000001421, 35.00000000000000000 ) ) ;
#8757 = ORIENTED_EDGE ( 'NONE', *, *, #8036, .F. ) ;
#8758 = ORIENTED_EDGE ( 'NONE', *, *, #15969, .T. ) ;
#8759 = DIRECTION ( 'NONE',  ( -0.9876526153536341335, -0.1566598588826327021, 0.000000000000000000 ) ) ;
#8760 = DIRECTION ( 'NONE',  ( 0.000000000000000000, 0.000000000000000000, 1.000000000000000000 ) ) ;
#8761 = EDGE_CURVE ( 'NONE', #14798, #17742, #13838, .T. ) ;
#8762 = FACE_OUTER_BOUND ( 'NONE', #4690, .T. ) ;
#8763 = VECTOR ( 'NONE', #2226, 1000.000000000000000 ) ;
#8764 = CIRCLE ( 'NONE', #15423, 1.500000000000000888 ) ;
#8765 = CIRCLE ( 'NONE', #8163, 2.000000000000000000 ) ;
#8766 = ORIENTED_EDGE ( 'NONE', *, *, #3787, .T. ) ;
#8767 = CARTESIAN_POINT ( 'NONE',  ( -129.1404785418517918, -15.35070196317932911, 2.500000000000000000 ) ) ;
#8768 = ORIENTED_EDGE ( 'NONE', *, *, #10953, .T. ) ;
#8769 = MANIFOLD_SOLID_BREP ( 'Move Face1', #18776 ) ;
#8770 = DIRECTION ( 'NONE',  ( -0.1566598588826321192, 0.9876526153536342445, 7.798540720466731404E-17 ) ) ;
#8771 = AXIS2_PLACEMENT_3D ( 'NONE', #8938, #14716, #17881 ) ;
#8772 = CARTESIAN_POINT ( 'NONE',  ( -84.16561914167408531, -33.59999999999994458, 30.00000000000000000 ) ) ;
#8773 =( NAMED_UNIT ( * ) SI_UNIT ( $, .STERADIAN. ) SOLID_ANGLE_UNIT ( ) );
#8774 = ORIENTED_EDGE ( 'NONE', *, *, #14007, .F. ) ;
#8775 = AXIS2_PLACEMENT_3D ( 'NONE', #2108, #4759, #16151 ) ;
#8776 = ADVANCED_FACE ( 'NONE', ( #5813 ), #5523, .F. ) ;
#8777 = CARTESIAN_POINT ( 'NONE',  ( -89.99999999999998579, -35.00000000000001421, -2.500000000000000000 ) ) ;
#8778 = CIRCLE ( 'NONE', #3628, 1.499999999999999556 ) ;
#8779 = CARTESIAN_POINT ( 'NONE',  ( -33.16810284049710589, -83.21632480446696434, 21.65063509461101532 ) ) ;
#8780 = CARTESIAN_POINT ( 'NONE',  ( -7.818242838216901802, -16.42739403096095074, -8.660254037844380193 ) ) ;
#8781 = CARTESIAN_POINT ( 'NONE',  ( -129.1404785418517918, -2.850701963179328668, 9.951701414186818625E-16 ) ) ;
#8782 = EDGE_LOOP ( 'NONE', ( #6073, #6437, #5751, #18488, #17258 ) ) ;
#8783 = ORIENTED_EDGE ( 'NONE', *, *, #17715, .T. ) ;
#8784 = LINE ( 'NONE', #5938, #17002 ) ;
#8785 = ORIENTED_EDGE ( 'NONE', *, *, #16543, .F. ) ;
#8786 = EDGE_CURVE ( 'NONE', #12053, #16372, #17566, .T. ) ;
#8787 = AXIS2_PLACEMENT_3D ( 'NONE', #4336, #11520, #17533 ) ;
#8788 = VECTOR ( 'NONE', #4900, 1000.000000000000000 ) ;
#8789 = VERTEX_POINT ( 'NONE', #189 ) ;
#8790 = CIRCLE ( 'NONE', #4551, 150.0000000000000000 ) ;
#8791 = ORIENTED_EDGE ( 'NONE', *, *, #15456, .F. ) ;
#8792 = DIRECTION ( 'NONE',  ( 1.000000000000000000, 0.000000000000000000, 0.000000000000000000 ) ) ;
#8793 = ORIENTED_EDGE ( 'NONE', *, *, #5620, .T. ) ;
#8794 = CARTESIAN_POINT ( 'NONE',  ( -17.69476899175320739, -17.99399261978727083, -8.660254037844380193 ) ) ;
#8795 = DIRECTION ( 'NONE',  ( 0.000000000000000000, -1.000000000000000000, 0.000000000000000000 ) ) ;
#8796 = EDGE_CURVE ( 'NONE', #450, #3169, #1014, .T. ) ;
#8797 = ORIENTED_EDGE ( 'NONE', *, *, #10923, .T. ) ;
#8798 = CARTESIAN_POINT ( 'NONE',  ( -45.51376053241749986, -85.17457304049983691, -17.32050807568878525 ) ) ;
#8799 = CYLINDRICAL_SURFACE ( 'NONE', #1768, 1.500000000000001554 ) ;
#8800 = AXIS2_PLACEMENT_3D ( 'NONE', #5257, #9231, #15204 ) ;
#8801 = DIRECTION ( 'NONE',  ( -0.9876526153536341335, -0.1566598588826327021, 0.000000000000000000 ) ) ;
#8802 = ORIENTED_EDGE ( 'NONE', *, *, #14862, .T. ) ;
#8803 = CIRCLE ( 'NONE', #1835, 1.499999999999999556 ) ;
#8804 = CARTESIAN_POINT ( 'NONE',  ( 0.000000000000000000, 0.000000000000000000, 35.00000000000000000 ) ) ;
#8805 = EDGE_CURVE ( 'NONE', #8207, #7506, #5846, .T. ) ;
#8806 = EDGE_CURVE ( 'NONE', #14356, #1673, #2507, .T. ) ;
#8807 = CARTESIAN_POINT ( 'NONE',  ( -6.995308533625909320, -79.06483854407721878, 4.330127018922213189 ) ) ;
#8808 = DIRECTION ( 'NONE',  ( 0.1566598588826321470, -0.9876526153536342445, 5.026083453879674093E-18 ) ) ;
#8809 = EDGE_CURVE ( 'NONE', #4130, #8275, #2215, .T. ) ;
#8810 = VERTEX_POINT ( 'NONE', #4450 ) ;
#8811 = EDGE_CURVE ( 'NONE', #10439, #14890, #15530, .T. ) ;
#8812 = CIRCLE ( 'NONE', #17921, 1.500000000000000888 ) ;
#8813 = VERTEX_POINT ( 'NONE', #1271 ) ;
#8814 = DIRECTION ( 'NONE',  ( -0.1566598588826321747, 0.9876526153536343555, 0.000000000000000000 ) ) ;
#8815 = EDGE_CURVE ( 'NONE', #7859, #4208, #9173, .T. ) ;
#8816 = EDGE_LOOP ( 'NONE', ( #1701, #4073, #845, #11378 ) ) ;
#8817 = EDGE_CURVE ( 'NONE', #8822, #9530, #5237, .T. ) ;
#8818 = ORIENTED_EDGE ( 'NONE', *, *, #13305, .F. ) ;
#8819 = CIRCLE ( 'NONE', #45, 1.500000000000000000 ) ;
#8820 = CARTESIAN_POINT ( 'NONE',  ( -79.30363509306917535, 32.43333333333333002, -24.99999999999999289 ) ) ;
#8821 = DIRECTION ( 'NONE',  ( 0.000000000000000000, 0.000000000000000000, 1.000000000000000000 ) ) ;
#8822 = VERTEX_POINT ( 'NONE', #2662 ) ;
#8823 = CIRCLE ( 'NONE', #7656, 1.499999999999999556 ) ;
#8824 = DIRECTION ( 'NONE',  ( -0.1566598588826321192, 0.9876526153536342445, 7.798540720466731404E-17 ) ) ;
#8825 = CIRCLE ( 'NONE', #11231, 1.500000000000000888 ) ;
#8826 = DIRECTION ( 'NONE',  ( 1.000000000000000000, 5.329070518200749027E-15, -2.631994239413086031E-16 ) ) ;
#8827 = DIRECTION ( 'NONE',  ( -0.9868632313631133801, 0.1615579233078772714, 2.699728182682517290E-16 ) ) ;
#8828 = ORIENTED_EDGE ( 'NONE', *, *, #5760, .F. ) ;
#8829 = VECTOR ( 'NONE', #14395, 1000.000000000000000 ) ;
#8830 = AXIS2_PLACEMENT_3D ( 'NONE', #14441, #13104, #135 ) ;
#8831 = EDGE_CURVE ( 'NONE', #16655, #7156, #3113, .T. ) ;
#8832 = ORIENTED_EDGE ( 'NONE', *, *, #12362, .T. ) ;
#8833 = FACE_OUTER_BOUND ( 'NONE', #11116, .T. ) ;
#8834 = DIRECTION ( 'NONE',  ( -0.1566598588826321192, 0.9876526153536342445, 7.798540720466730171E-17 ) ) ;
#8835 = CARTESIAN_POINT ( 'NONE',  ( -65.37641414873195345, -43.03264333350145421, 20.00000000000001421 ) ) ;
#8837 = EDGE_CURVE ( 'NONE', #10533, #11499, #13392, .T. ) ;
#8836 = CARTESIAN_POINT ( 'NONE',  ( -72.01566283620284992, -26.61028485833200818, -17.32050807568878170 ) ) ;
#8838 = AXIS2_PLACEMENT_3D ( 'NONE', #1985, #2178, #9475 ) ;
#8839 = EDGE_LOOP ( 'NONE', ( #3417, #18407, #7087, #5630 ) ) ;
#8840 = ORIENTED_EDGE ( 'NONE', *, *, #4880, .T. ) ;
#8841 = EDGE_CURVE ( 'NONE', #17674, #8596, #4921, .T. ) ;
#8842 = AXIS2_PLACEMENT_3D ( 'NONE', #12883, #8723, #8639 ) ;
#8843 = CARTESIAN_POINT ( 'NONE',  ( -5.513829610595458064, -78.82984875575326100, 21.65063509461100821 ) ) ;
#8844 = EDGE_LOOP ( 'NONE', ( #16859, #16203, #1711, #4537 ) ) ;
#8845 = ORIENTED_EDGE ( 'NONE', *, *, #11598, .F. ) ;
#8846 = CARTESIAN_POINT ( 'NONE',  ( -11.76885329963143079, -17.05403346649147878, 21.65063509461101532 ) ) ;
#8847 = ORIENTED_EDGE ( 'NONE', *, *, #16796, .F. ) ;
#8848 = CARTESIAN_POINT ( 'NONE',  ( -66.08974714408108753, -25.67032570503622679, 12.99038105676661736 ) ) ;
#8849 = CONICAL_SURFACE ( 'NONE', #17954, 12.74754878398197633, 0.01745329251994333364 ) ;
#8850 = CARTESIAN_POINT ( 'NONE',  ( -58.68235252892886678, -24.49537676341648407, 1.908195823574487804E-14 ) ) ;
#8851 = EDGE_LOOP ( 'NONE', ( #4513, #706 ) ) ;
#8852 = ORIENTED_EDGE ( 'NONE', *, *, #12246, .T. ) ;
#8853 = AXIS2_PLACEMENT_3D ( 'NONE', #14183, #2333, #8125 ) ;
#8854 = ORIENTED_EDGE ( 'NONE', *, *, #9492, .T. ) ;
#8855 = CARTESIAN_POINT ( 'NONE',  ( -49.95819730150881099, -85.87954240547168183, 4.330127018922213189 ) ) ;
#8856 = DIRECTION ( 'NONE',  ( 0.000000000000000000, 0.000000000000000000, 1.000000000000000000 ) ) ;
#8857 = DIRECTION ( 'NONE',  ( -0.1566598588826321747, 0.9876526153536343555, 0.000000000000000000 ) ) ;
#8858 = CARTESIAN_POINT ( 'NONE',  ( -84.16561914167411373, 33.60000000000000142, 30.00000000000000000 ) ) ;
#8859 = CARTESIAN_POINT ( 'NONE',  ( -71.56969528596198415, 45.66791243518527921, -3.731434853903564886 ) ) ;
#8860 = EDGE_LOOP ( 'NONE', ( #10110, #6598, #16429, #4060 ) ) ;
#8861 = ORIENTED_EDGE ( 'NONE', *, *, #10748, .F. ) ;
#8862 = DIRECTION ( 'NONE',  ( -0.1566598588826321192, 0.9876526153536342445, 7.798540720466730171E-17 ) ) ;
#8863 = CARTESIAN_POINT ( 'NONE',  ( -59.67000514428248437, -24.65203662229912140, 4.330127018922218518 ) ) ;
#8864 = ADVANCED_FACE ( 'NONE', ( #4167 ), #14606, .F. ) ;
#8865 = DIRECTION ( 'NONE',  ( -0.1566598588826321747, 0.9876526153536343555, 0.000000000000000000 ) ) ;
#8866 = COLOUR_RGB ( '', 0.08235294, 0.09019608, 0.10196078) ;
#8867 = ORIENTED_EDGE ( 'NONE', *, *, #8036, .T. ) ;
#8868 = DIRECTION ( 'NONE',  ( -0.1566598588826321192, 0.9876526153536342445, 7.798540720466731404E-17 ) ) ;
#8869 = DIRECTION ( 'NONE',  ( -0.1566598588826321192, 0.9876526153536342445, 7.798540720466730171E-17 ) ) ;
#8870 = EDGE_CURVE ( 'NONE', #6775, #15850, #10541, .T. ) ;
#8871 = LINE ( 'NONE', #10368, #5793 ) ;
#8872 = DIRECTION ( 'NONE',  ( 0.000000000000000000, 0.000000000000000000, 1.000000000000000000 ) ) ;
#8873 = CARTESIAN_POINT ( 'NONE',  ( -5.000000000000000000, 6.123233995736766282E-16, 30.00000000000000000 ) ) ;
#8874 = SURFACE_STYLE_USAGE ( .BOTH. , #13583 ) ;
#8875 = AXIS2_PLACEMENT_3D ( 'NONE', #9098, #8994, #674 ) ;
#8876 = CARTESIAN_POINT ( 'NONE',  ( -3.578159390066044665, -20.81734760163988440, 8.660254037844412167 ) ) ;
#8877 = CARTESIAN_POINT ( 'NONE',  ( 0.000000000000000000, 0.000000000000000000, 25.00000000000000000 ) ) ;
#8878 = DIRECTION ( 'NONE',  ( -0.9876526153536336894, -0.1566598588826349503, 0.000000000000000000 ) ) ;
#8879 = DIRECTION ( 'NONE',  ( -0.1566598588826321192, 0.9876526153536342445, 7.798540720466730171E-17 ) ) ;
#8880 = ORIENTED_EDGE ( 'NONE', *, *, #9267, .T. ) ;
#8881 = ORIENTED_EDGE ( 'NONE', *, *, #945, .T. ) ;
#8882 = DIRECTION ( 'NONE',  ( 1.000000000000000000, 0.000000000000000000, 0.000000000000000000 ) ) ;
#8883 = ORIENTED_EDGE ( 'NONE', *, *, #14862, .F. ) ;
#8884 = CYLINDRICAL_SURFACE ( 'NONE', #3922, 1.500000000000001554 ) ;
#8885 = VERTEX_POINT ( 'NONE', #4820 ) ;
#8886 = AXIS2_PLACEMENT_3D ( 'NONE', #14756, #2053, #4793 ) ;
#8887 = EDGE_CURVE ( 'NONE', #15855, #9188, #7088, .T. ) ;
#8888 = CARTESIAN_POINT ( 'NONE',  ( -40.08167114797252140, -84.31294381664535820, -12.99038105676658539 ) ) ;
#8889 = DIRECTION ( 'NONE',  ( -1.000000000000000000, 0.000000000000000000, 0.000000000000000000 ) ) ;
#8890 = FACE_OUTER_BOUND ( 'NONE', #15837, .T. ) ;
#8891 = DIRECTION ( 'NONE',  ( -0.1566598588826321192, 0.9876526153536342445, 7.798540720466731404E-17 ) ) ;
#8892 = DIRECTION ( 'NONE',  ( -0.1566598588826321192, 0.9876526153536342445, 7.798540720466730171E-17 ) ) ;
#8893 = DIRECTION ( 'NONE',  ( -0.9876526153536336894, -0.1566598588826349503, 0.000000000000000000 ) ) ;
#8894 = ADVANCED_FACE ( 'NONE', ( #14873 ), #392, .F. ) ;
#8895 = CARTESIAN_POINT ( 'NONE',  ( -4.565812005419673802, -20.97400746052251108, 4.330127018922214077 ) ) ;
#8896 = DIRECTION ( 'NONE',  ( -0.9876526153536344665, -0.1566598588826304539, 0.000000000000000000 ) ) ;
#8897 = FACE_BOUND ( 'NONE', #13098, .T. ) ;
#8898 = DIRECTION ( 'NONE',  ( -0.9876526153536341335, -0.1566598588826327021, 0.000000000000000000 ) ) ;
#8900 = VERTEX_POINT ( 'NONE', #16129 ) ;
#8899 = CARTESIAN_POINT ( 'NONE',  ( -84.20693962813486166, 32.64562644091790844, -35.00000000000000000 ) ) ;
#8901 = VERTEX_POINT ( 'NONE', #7685 ) ;
#8902 = CARTESIAN_POINT ( 'NONE',  ( -128.1404785157144204, 9.631497293019405603, 2.500000000000000000 ) ) ;
#8903 = ORIENTED_EDGE ( 'NONE', *, *, #11599, .T. ) ;
#8904 = ORIENTED_EDGE ( 'NONE', *, *, #17436, .F. ) ;
#8905 = DIRECTION ( 'NONE',  ( -0.1566598588826321192, 0.9876526153536342445, 7.798540720466731404E-17 ) ) ;
#8906 = DIRECTION ( 'NONE',  ( -0.9876526153536341335, -0.1566598588826327021, 0.000000000000000000 ) ) ;
#8907 = VERTEX_POINT ( 'NONE', #1981 ) ;
#8908 = EDGE_CURVE ( 'NONE', #16999, #1829, #12805, .T. ) ;
#8909 = EDGE_CURVE ( 'NONE', #10566, #1820, #1320, .T. ) ;
#8910 = CARTESIAN_POINT ( 'NONE',  ( 11.77009115809307715, -76.08830122530719109, 9.226938858386234556E-15 ) ) ;
#8911 = EDGE_CURVE ( 'NONE', #8822, #16032, #12196, .T. ) ;
#8912 = UNCERTAINTY_MEASURE_WITH_UNIT (LENGTH_MEASURE( 1.000000000000000082E-05 ), #3872, 'distance_accuracy_value', 'NONE');
#8913 = CARTESIAN_POINT ( 'NONE',  ( 11.59211860341529565, 6.314490184041233967, 20.00000000000000000 ) ) ;
#8914 = AXIS2_PLACEMENT_3D ( 'NONE', #11876, #6137, #17628 ) ;
#8915 = EDGE_LOOP ( 'NONE', ( #2321, #2538 ) ) ;
#8916 = DIRECTION ( 'NONE',  ( 1.000000000000000000, 0.000000000000000000, 0.000000000000000000 ) ) ;
#8917 = ORIENTED_EDGE ( 'NONE', *, *, #15843, .T. ) ;
#8918 = DIRECTION ( 'NONE',  ( -0.1566598588826321747, 0.9876526153536343555, 0.000000000000000000 ) ) ;
#8919 = CARTESIAN_POINT ( 'NONE',  ( -46.54104815794897121, -27.63205146303434390, -17.32050807568878170 ) ) ;
#8920 = ORIENTED_EDGE ( 'NONE', *, *, #9657, .T. ) ;
#8921 = ORIENTED_EDGE ( 'NONE', *, *, #11384, .F. ) ;
#8922 = ORIENTED_EDGE ( 'NONE', *, *, #5614, .F. ) ;
#8923 = ORIENTED_EDGE ( 'NONE', *, *, #270, .F. ) ;
#8924 = DIRECTION ( 'NONE',  ( -0.1566598588826321747, 0.9876526153536343555, 0.000000000000000000 ) ) ;
#8925 = EDGE_LOOP ( 'NONE', ( #6216, #3576, #1176, #586 ) ) ;
#8926 = AXIS2_PLACEMENT_3D ( 'NONE', #11685, #14654, #8610 ) ;
#8927 = FACE_BOUND ( 'NONE', #14248, .T. ) ;
#8928 = EDGE_CURVE ( 'NONE', #7859, #11927, #7766, .T. ) ;
#8929 = ORIENTED_EDGE ( 'NONE', *, *, #572, .F. ) ;
#8930 = CARTESIAN_POINT ( 'NONE',  ( 2.058283315319403783, -14.86079544213463066, -8.660254037844383745 ) ) ;
#8931 = EDGE_CURVE ( 'NONE', #5315, #6912, #17072, .T. ) ;
#8932 = CARTESIAN_POINT ( 'NONE',  ( 2.000000000000000000, 2.449293598294706414E-16, 35.00000000000000000 ) ) ;
#8933 = ORIENTED_EDGE ( 'NONE', *, *, #11310, .F. ) ;
#8934 = FACE_BOUND ( 'NONE', #15571, .T. ) ;
#8935 = EDGE_CURVE ( 'NONE', #5645, #3917, #3387, .T. ) ;
#8936 = CARTESIAN_POINT ( 'NONE',  ( -15.39035576413176187, -80.39644734457957043, -21.65063509461098690 ) ) ;
#8937 = AXIS2_PLACEMENT_3D ( 'NONE', #16623, #422, #509 ) ;
#8938 = CARTESIAN_POINT ( 'NONE',  ( -31.52190560670403841, -20.18723064414411539, 4.330127018922218518 ) ) ;
#8939 = CARTESIAN_POINT ( 'NONE',  ( -126.1404785418517918, -15.29729532696464567, -2.500000000000000000 ) ) ;
#8940 = DIRECTION ( 'NONE',  ( -0.9876526153536341335, -0.1566598588826327021, 0.000000000000000000 ) ) ;
#8941 = VERTEX_POINT ( 'NONE', #476 ) ;
#8942 = ORIENTED_EDGE ( 'NONE', *, *, #13395, .T. ) ;
#8943 = FACE_BOUND ( 'NONE', #2997, .T. ) ;
#8944 = FACE_OUTER_BOUND ( 'NONE', #17638, .T. ) ;
#8945 = DIRECTION ( 'NONE',  ( -0.1566598588826321192, 0.9876526153536342445, 7.798540720466731404E-17 ) ) ;
#8946 = ORIENTED_EDGE ( 'NONE', *, *, #16346, .F. ) ;
#8947 = CARTESIAN_POINT ( 'NONE',  ( -26.58364252993588650, -19.40393134973095002, -21.65063509461097979 ) ) ;
#8948 = ORIENTED_EDGE ( 'NONE', *, *, #5639, .F. ) ;
#8949 = AXIS2_PLACEMENT_3D ( 'NONE', #8438, #7041, #12786 ) ;
#8950 = CARTESIAN_POINT ( 'NONE',  ( -172.7326993491721225, 43.83249341393818810, 9.951701414186830458E-16 ) ) ;
#8951 = DIRECTION ( 'NONE',  ( -0.9876526153536336894, -0.1566598588826349503, 0.000000000000000000 ) ) ;
#8952 = EDGE_CURVE ( 'NONE', #2351, #3748, #12102, .T. ) ;
#8953 = EDGE_CURVE ( 'NONE', #299, #14468, #18621, .T. ) ;
#8954 = CARTESIAN_POINT ( 'NONE',  ( -18.39294862037050393, -23.16724548487935564, 8.660254037844417496 ) ) ;
#8955 =( NAMED_UNIT ( * ) SI_UNIT ( $, .STERADIAN. ) SOLID_ANGLE_UNIT ( ) );
#8956 = DIRECTION ( 'NONE',  ( -0.1566598588826321192, 0.9876526153536342445, 7.798540720466730171E-17 ) ) ;
#8957 = ORIENTED_EDGE ( 'NONE', *, *, #12842, .F. ) ;
#8958 = DIRECTION ( 'NONE',  ( 0.000000000000000000, 0.000000000000000000, -1.000000000000000000 ) ) ;
#8959 = EDGE_CURVE ( 'NONE', #1993, #14599, #14916, .T. ) ;
#8960 = CIRCLE ( 'NONE', #806, 1.500000000000000888 ) ;
#8961 = ORIENTED_EDGE ( 'NONE', *, *, #4092, .T. ) ;
#8962 = ORIENTED_EDGE ( 'NONE', *, *, #7331, .T. ) ;
#8963 = AXIS2_PLACEMENT_3D ( 'NONE', #7135, #11361, #1439 ) ;
#8964 = DIRECTION ( 'NONE',  ( -0.000000000000000000, -0.000000000000000000, -1.000000000000000000 ) ) ;
#8965 = EDGE_LOOP ( 'NONE', ( #8828, #13645, #16545, #2460 ) ) ;
#8966 = LINE ( 'NONE', #14754, #14565 ) ;
#8967 = CARTESIAN_POINT ( 'NONE',  ( -38.14600092744310444, -26.30044266253198160, 17.32050807568881723 ) ) ;
#8968 = AXIS2_PLACEMENT_3D ( 'NONE', #14089, #1133, #12651 ) ;
#8969 = LINE ( 'NONE', #15903, #17031 ) ;
#8970 = DIRECTION ( 'NONE',  ( -0.9876526153536341335, -0.1566598588826327021, 0.000000000000000000 ) ) ;
#8971 = EDGE_CURVE ( 'NONE', #898, #7429, #15215, .T. ) ;
#8972 = DIRECTION ( 'NONE',  ( -0.1566598588826321192, 0.9876526153536342445, 7.798540720466730171E-17 ) ) ;
#8973 = EDGE_LOOP ( 'NONE', ( #9559, #7164 ) ) ;
#8974 = CARTESIAN_POINT ( 'NONE',  ( -59.38053215754615621, -29.66862962850855823, 8.660254037844417496 ) ) ;
#8975 = VECTOR ( 'NONE', #2048, 1000.000000000000000 ) ;
#8976 = AXIS2_PLACEMENT_3D ( 'NONE', #8233, #2536, #14001 ) ;
#8977 = DIRECTION ( 'NONE',  ( -0.9876526153536341335, -0.1566598588826327576, 0.000000000000000000 ) ) ;
#8978 = DIRECTION ( 'NONE',  ( 0.000000000000000000, 0.000000000000000000, 1.000000000000000000 ) ) ;
#8979 = EDGE_CURVE ( 'NONE', #113, #4333, #13525, .T. ) ;
#8981 = ORIENTED_EDGE ( 'NONE', *, *, #7635, .T. ) ;
#8980 = CARTESIAN_POINT ( 'NONE',  ( -48.02252708097939404, -27.86704125135830523, 17.32050807568881723 ) ) ;
#8982 = ORIENTED_EDGE ( 'NONE', *, *, #8453, .F. ) ;
#8983 = CYLINDRICAL_SURFACE ( 'NONE', #14740, 1.500000000000001554 ) ;
#8984 = CIRCLE ( 'NONE', #14130, 145.0000000000000284 ) ;
#8985 = AXIS2_PLACEMENT_3D ( 'NONE', #15111, #8298, #16842 ) ;
#8986 = VERTEX_POINT ( 'NONE', #15056 ) ;
#8987 = ADVANCED_FACE ( 'NONE', ( #7493 ), #1708, .F. ) ;
#8988 = CIRCLE ( 'NONE', #4736, 1.500000000000000888 ) ;
#8989 = EDGE_LOOP ( 'NONE', ( #17085, #14663, #7630, #18618 ) ) ;
#8990 = DIRECTION ( 'NONE',  ( -0.1566598588826321192, 0.9876526153536342445, 7.798540720466730171E-17 ) ) ;
#8991 = VERTEX_POINT ( 'NONE', #284 ) ;
#8992 = DIRECTION ( 'NONE',  ( 1.000000000000000000, 0.000000000000000000, 0.000000000000000000 ) ) ;
#8993 = CIRCLE ( 'NONE', #2943, 3.000000000000004441 ) ;
#8994 = DIRECTION ( 'NONE',  ( -0.1566598588826321747, 0.9876526153536343555, 0.000000000000000000 ) ) ;
#8995 = ORIENTED_EDGE ( 'NONE', *, *, #14781, .T. ) ;
#8996 = FACE_OUTER_BOUND ( 'NONE', #8670, .T. ) ;
#8997 = DIRECTION ( 'NONE',  ( -1.000000000000000000, 0.000000000000000000, 0.000000000000000000 ) ) ;
#8998 = ADVANCED_FACE ( 'NONE', ( #17670 ), #4639, .F. ) ;
#8999 = PRODUCT_DEFINITION_FORMATION_WITH_SPECIFIED_SOURCE ( 'ANY', '', #3936, .NOT_KNOWN. ) ;
#9000 = CARTESIAN_POINT ( 'NONE',  ( -30.73860631229088725, -25.12549372091224598, 12.99038105676661736 ) ) ;
#9001 = ORIENTED_EDGE ( 'NONE', *, *, #8156, .T. ) ;
#9002 = CIRCLE ( 'NONE', #3241, 1.499999999999999556 ) ;
#9003 = CARTESIAN_POINT ( 'NONE',  ( -312.1404785418517918, -2.850701963179328668, 9.951701414186818625E-16 ) ) ;
#9004 = EDGE_LOOP ( 'NONE', ( #18214, #3807, #1697, #11052 ) ) ;
#9005 = EDGE_CURVE ( 'NONE', #10290, #18222, #1620, .T. ) ;
#9006 = DIRECTION ( 'NONE',  ( -0.000000000000000000, -0.000000000000000000, 1.000000000000000000 ) ) ;
#9007 = CARTESIAN_POINT ( 'NONE',  ( -26.74836084069850983, -82.19803572172985184, -12.99038105676658539 ) ) ;
#9008 = AXIS2_PLACEMENT_3D ( 'NONE', #7218, #10397, #12962 ) ;
#9009 = EDGE_LOOP ( 'NONE', ( #2717, #12509 ) ) ;
#9010 = EDGE_LOOP ( 'NONE', ( #13450, #8671, #12348, #15986 ) ) ;
#9011 = EDGE_CURVE ( 'NONE', #12973, #6731, #5100, .T. ) ;
#9012 = ORIENTED_EDGE ( 'NONE', *, *, #17803, .F. ) ;
#9013 = ORIENTED_EDGE ( 'NONE', *, *, #14350, .F. ) ;
#9014 = DIRECTION ( 'NONE',  ( -0.9876526153536336894, -0.1566598588826349503, 0.000000000000000000 ) ) ;
#9015 = CIRCLE ( 'NONE', #10569, 1.500000000000000444 ) ;
#9016 = EDGE_LOOP ( 'NONE', ( #12204, #11639, #14702, #2116 ) ) ;
#9017 = FACE_BOUND ( 'NONE', #9443, .T. ) ;
#9018 = AXIS2_PLACEMENT_3D ( 'NONE', #583, #1809, #7598 ) ;
#9019 = ORIENTED_EDGE ( 'NONE', *, *, #2037, .T. ) ;
#9020 = DIRECTION ( 'NONE',  ( -0.9876526153536336894, -0.1566598588826350336, 0.000000000000000000 ) ) ;
#9021 = EDGE_LOOP ( 'NONE', ( #11958, #1038 ) ) ;
#9022 = EDGE_LOOP ( 'NONE', ( #12260, #13854, #16773, #13366 ) ) ;
#9023 = EDGE_CURVE ( 'NONE', #8348, #18596, #6153, .T. ) ;
#9024 = AXIS2_PLACEMENT_3D ( 'NONE', #4311, #17227, #15788 ) ;
#9025 = ORIENTED_EDGE ( 'NONE', *, *, #5488, .T. ) ;
#9026 = VECTOR ( 'NONE', #15492, 1000.000000000000000 ) ;
#9027 = LINE ( 'NONE', #14997, #310 ) ;
#9028 = AXIS2_PLACEMENT_3D ( 'NONE', #14164, #17123, #15669 ) ;
#9029 = CARTESIAN_POINT ( 'NONE',  ( -27.28182215855319015, -24.57718421482303484, 12.99038105676661736 ) ) ;
#9030 = EDGE_CURVE ( 'NONE', #13292, #2965, #2517, .T. ) ;
#9031 = DIRECTION ( 'NONE',  ( -0.9876526153536336894, -0.1566598588826349503, 0.000000000000000000 ) ) ;
#9032 = CARTESIAN_POINT ( 'NONE',  ( -55.39028668595378946, -86.74117162932616054, 8.660254037844412167 ) ) ;
#9033 = EDGE_CURVE ( 'NONE', #10329, #5781, #16758, .T. ) ;
#9034 = CARTESIAN_POINT ( 'NONE',  ( -31.72625892764450839, -25.28215357979487266, 17.32050807568881723 ) ) ;
#9035 = ORIENTED_EDGE ( 'NONE', *, *, #6582, .T. ) ;
#9036 = ORIENTED_EDGE ( 'NONE', *, *, #16993, .T. ) ;
#9037 = CARTESIAN_POINT ( 'NONE',  ( -20.86208015875458344, -23.55889513208593655, 4.330127018922217630 ) ) ;
#9038 = EDGE_CURVE ( 'NONE', #7926, #7658, #16885, .T. ) ;
#9039 = ADVANCED_FACE ( 'NONE', ( #18336 ), #5304, .F. ) ;
#9040 = CARTESIAN_POINT ( 'NONE',  ( -50.28730529842300001, -23.16376796291412177, 17.32050807568881723 ) ) ;
#9041 = AXIS2_PLACEMENT_3D ( 'NONE', #12806, #17463, #4069 ) ;
#9042 = AXIS2_PLACEMENT_3D ( 'NONE', #6092, #17473, #13172 ) ;
#9043 = EDGE_LOOP ( 'NONE', ( #2857, #4442, #15314, #12970 ) ) ;
#9044 = CARTESIAN_POINT ( 'NONE',  ( -24.27922930231443743, -81.80638607452327449, 17.32050807568881368 ) ) ;
#9045 = AXIS2_PLACEMENT_3D ( 'NONE', #15538, #1158, #15723 ) ;
#9046 = AXIS2_PLACEMENT_3D ( 'NONE', #4981, #15233, #10758 ) ;
#9047 = CARTESIAN_POINT ( 'NONE',  ( -19.38060123572412863, -23.32390534376198232, -12.99038105676658006 ) ) ;
#9048 = DIRECTION ( 'NONE',  ( -0.1566598588826321192, 0.9876526153536342445, 7.798540720466731404E-17 ) ) ;
#9049 = SHAPE_REPRESENTATION_RELATIONSHIP ( 'NONE' , 'NONE' ,  #10585, #16340 ) ;
#9050 = VERTEX_POINT ( 'NONE', #1064 ) ;
#9051 = CIRCLE ( 'NONE', #8470, 1.500000000000000888 ) ;
#9052 = DIRECTION ( 'NONE',  ( -0.9876526153536341335, -0.1566598588826327576, 0.000000000000000000 ) ) ;
#9053 = AXIS2_PLACEMENT_3D ( 'NONE', #9858, #3112, #1530 ) ;
#9054 = DIRECTION ( 'NONE',  ( 1.000000000000000000, 0.000000000000000000, 0.000000000000000000 ) ) ;
#9055 = AXIS2_PLACEMENT_3D ( 'NONE', #10183, #3162, #11413 ) ;
#9056 = EDGE_CURVE ( 'NONE', #2319, #5366, #1907, .T. ) ;
#9057 = ORIENTED_EDGE ( 'NONE', *, *, #807, .F. ) ;
#9058 = VERTEX_POINT ( 'NONE', #3571 ) ;
#9059 = DIRECTION ( 'NONE',  ( -0.1566598588826321747, 0.9876526153536343555, 0.000000000000000000 ) ) ;
#9060 = VECTOR ( 'NONE', #5581, 1000.000000000000000 ) ;
#9061 = AXIS2_PLACEMENT_3D ( 'NONE', #2128, #13677, #4872 ) ;
#9062 = EDGE_LOOP ( 'NONE', ( #8421, #16531 ) ) ;
#9064 = ORIENTED_EDGE ( 'NONE', *, *, #18134, .F. ) ;
#9063 = DIRECTION ( 'NONE',  ( 0.9876526153536342445, 0.1566598588826321192, -2.851797552515346363E-16 ) ) ;
#9065 = ORIENTED_EDGE ( 'NONE', *, *, #2240, .T. ) ;
#9066 = EDGE_CURVE ( 'NONE', #2189, #3917, #8579, .T. ) ;
#9067 = ORIENTED_EDGE ( 'NONE', *, *, #14539, .F. ) ;
#9068 = CIRCLE ( 'NONE', #9697, 1.500000000000000888 ) ;
#9069 = DIRECTION ( 'NONE',  ( -0.1566598588826321192, 0.9876526153536342445, 7.798540720466730171E-17 ) ) ;
#9070 = DIRECTION ( 'NONE',  ( -1.000000000000000000, -0.000000000000000000, -0.000000000000000000 ) ) ;
#9071 = CIRCLE ( 'NONE', #15119, 1.500000000000000444 ) ;
#9072 = DIRECTION ( 'NONE',  ( -0.1566598588826321192, 0.9876526153536342445, 7.798540720466730171E-17 ) ) ;
#9073 =( REPRESENTATION_RELATIONSHIP ('NONE','NONE', #7353, #5397 ) REPRESENTATION_RELATIONSHIP_WITH_TRANSFORMATION ( #10075 )SHAPE_REPRESENTATION_RELATIONSHIP( ) );
#9074 = FACE_OUTER_BOUND ( 'NONE', #8165, .T. ) ;
#9075 = LINE ( 'NONE', #14758, #11546 ) ;
#9076 = PRODUCT ( 'Lower Hopper Receiver Handle Arm', 'Lower Hopper Receiver Handle Arm', '', ( #4199 ) ) ;
#9077 = DIRECTION ( 'NONE',  ( -0.1566598588826321747, 0.9876526153536343555, 0.000000000000000000 ) ) ;
#9078 = DIRECTION ( 'NONE',  ( 0.000000000000000000, 0.000000000000000000, 1.000000000000000000 ) ) ;
#9079 = AXIS2_PLACEMENT_3D ( 'NONE', #6439, #15030, #5070 ) ;
#9080 = FACE_OUTER_BOUND ( 'NONE', #8844, .T. ) ;
#9081 = VECTOR ( 'NONE', #12991, 1000.000000000000000 ) ;
#9083 = ORIENTED_EDGE ( 'NONE', *, *, #8427, .T. ) ;
#9082 = DIRECTION ( 'NONE',  ( -0.000000000000000000, -0.000000000000000000, -1.000000000000000000 ) ) ;
#9084 = VECTOR ( 'NONE', #320, 1000.000000000000000 ) ;
#9085 = ORIENTED_EDGE ( 'NONE', *, *, #9203, .F. ) ;
#9086 = DIRECTION ( 'NONE',  ( 0.000000000000000000, 0.000000000000000000, 1.000000000000000000 ) ) ;
#9087 = AXIS2_PLACEMENT_3D ( 'NONE', #18594, #15507, #7175 ) ;
#9088 = VERTEX_POINT ( 'NONE', #2175 ) ;
#9089 = EDGE_CURVE ( 'NONE', #7880, #2300, #4010, .T. ) ;
#9090 = EDGE_LOOP ( 'NONE', ( #8120, #5666 ) ) ;
#9091 = LINE ( 'NONE', #7490, #11381 ) ;
#9092 = ADVANCED_FACE ( 'NONE', ( #12288 ), #2352, .F. ) ;
#9093 = ORIENTED_EDGE ( 'NONE', *, *, #3482, .F. ) ;
#9094 = CYLINDRICAL_SURFACE ( 'NONE', #12748, 2.000000000000001776 ) ;
#9095 = ORIENTED_EDGE ( 'NONE', *, *, #17417, .T. ) ;
#9096 = CIRCLE ( 'NONE', #643, 20.00000000000001066 ) ;
#9097 = EDGE_CURVE ( 'NONE', #13575, #18385, #11577, .T. ) ;
#9098 = CARTESIAN_POINT ( 'NONE',  ( -23.33121169713865584, -23.95054477929251036, 17.32050807568881723 ) ) ;
#9099 = AXIS2_PLACEMENT_3D ( 'NONE', #6428, #18002, #1953 ) ;
#9100 = CARTESIAN_POINT ( 'NONE',  ( -63.62061560569701157, -25.27867605782963878, -8.660254037844380193 ) ) ;
#9101 = UNCERTAINTY_MEASURE_WITH_UNIT (LENGTH_MEASURE( 1.000000000000000082E-05 ), #7650, 'distance_accuracy_value', 'NONE');
#9102 = AXIS2_PLACEMENT_3D ( 'NONE', #1491, #7184, #17514 ) ;
#9103 = CARTESIAN_POINT ( 'NONE',  ( -62.30385499342917655, -87.83779064150456861, 1.443110928631665584E-14 ) ) ;
#9104 = DIRECTION ( 'NONE',  ( 0.000000000000000000, 0.000000000000000000, 1.000000000000000000 ) ) ;
#9105 = VERTEX_POINT ( 'NONE', #861 ) ;
#9106 = FACE_BOUND ( 'NONE', #8164, .T. ) ;
#9107 = CIRCLE ( 'NONE', #961, 1.500000000000000888 ) ;
#9108 = CARTESIAN_POINT ( 'NONE',  ( -39.91695283720987675, -21.51883944464648835, 4.330127018922218518 ) ) ;
#9109 = VERTEX_POINT ( 'NONE', #3672 ) ;
#9110 = DIRECTION ( 'NONE',  ( -0.9876526153536341335, -0.1566598588826327021, 0.000000000000000000 ) ) ;
#9111 = VECTOR ( 'NONE', #10073, 1000.000000000000000 ) ;
#9112 = LINE ( 'NONE', #14980, #9945 ) ;
#9113 = EDGE_LOOP ( 'NONE', ( #10847, #17255 ) ) ;
#9114 = CIRCLE ( 'NONE', #337, 1.500000000000000888 ) ;
#9115 = ORIENTED_EDGE ( 'NONE', *, *, #2882, .F. ) ;
#9116 = EDGE_LOOP ( 'NONE', ( #8852, #5207 ) ) ;
#9117 = VERTEX_POINT ( 'NONE', #12666 ) ;
#9118 = ORIENTED_EDGE ( 'NONE', *, *, #8971, .F. ) ;
#9119 = DIRECTION ( 'NONE',  ( -0.9876526153536336894, -0.1566598588826349503, 0.000000000000000000 ) ) ;
#9120 = VECTOR ( 'NONE', #15565, 1000.000000000000000 ) ;
#9121 = VERTEX_POINT ( 'NONE', #5398 ) ;
#9122 = FACE_BOUND ( 'NONE', #705, .T. ) ;
#9123 = ADVANCED_BREP_SHAPE_REPRESENTATION ( '', ( #2480, #18772 ), #9301 ) ;
#9124 = EDGE_CURVE ( 'NONE', #6916, #17944, #13103, .T. ) ;
#9125 = PRESENTATION_STYLE_ASSIGNMENT (( #14899 ) ) ;
#9126 = ORIENTED_EDGE ( 'NONE', *, *, #14049, .F. ) ;
#9127 = CIRCLE ( 'NONE', #10920, 1.500000000000001332 ) ;
#9128 = AXIS2_PLACEMENT_3D ( 'NONE', #5422, #12314, #3781 ) ;
#9129 = ORIENTED_EDGE ( 'NONE', *, *, #16451, .F. ) ;
#9130 = DIRECTION ( 'NONE',  ( -0.3915338189555018222, -0.9201637183752250371, 0.000000000000000000 ) ) ;
#9131 = EDGE_CURVE ( 'NONE', #14764, #7636, #3714, .T. ) ;
#9132 = CIRCLE ( 'NONE', #6108, 1.499999999999999556 ) ;
#9133 = CARTESIAN_POINT ( 'NONE',  ( 6.338001773648100468, -76.94993044916168401, -12.99038105676658894 ) ) ;
#9134 = ADVANCED_FACE ( 'NONE', ( #15243 ), #13914, .F. ) ;
#9135 = DIRECTION ( 'NONE',  ( -0.1566598588826321747, 0.9876526153536343555, 0.000000000000000000 ) ) ;
#9136 = CYLINDRICAL_SURFACE ( 'NONE', #7538, 13.99999999999999822 ) ;
#9137 = AXIS2_PLACEMENT_3D ( 'NONE', #13099, #1646, #9977 ) ;
#9138 = CARTESIAN_POINT ( 'NONE',  ( -52.42732883989288695, -86.27119205267825919, 8.660254037844412167 ) ) ;
#9139 = CARTESIAN_POINT ( 'NONE',  ( -13.41505053342451426, -80.08312762681433128, 21.65063509461100821 ) ) ;
#9140 = ORIENTED_EDGE ( 'NONE', *, *, #4314, .T. ) ;
#9141 = VERTEX_POINT ( 'NONE', #16983 ) ;
#9142 = CARTESIAN_POINT ( 'NONE',  ( -36.66452200441265319, -26.06545287420802737, 8.660254037844417496 ) ) ;
#9143 = DIRECTION ( 'NONE',  ( -1.000000000000000000, 0.000000000000000000, 0.000000000000000000 ) ) ;
#9144 = DIRECTION ( 'NONE',  ( -0.9876526153536336894, -0.1566598588826349503, 0.000000000000000000 ) ) ;
#9145 = VECTOR ( 'NONE', #11752, 1000.000000000000000 ) ;
#9146 = VERTEX_POINT ( 'NONE', #8337 ) ;
#9147 = ORIENTED_EDGE ( 'NONE', *, *, #9539, .T. ) ;
#9148 = VERTEX_POINT ( 'NONE', #966 ) ;
#9149 = DIRECTION ( 'NONE',  ( -0.1566598588826321192, 0.9876526153536342445, 7.798540720466730171E-17 ) ) ;
#9150 = VECTOR ( 'NONE', #3550, 1000.000000000000000 ) ;
#9151 = FACE_BOUND ( 'NONE', #6352, .T. ) ;
#9152 = EDGE_CURVE ( 'NONE', #4488, #7880, #3954, .T. ) ;
#9153 = EDGE_CURVE ( 'NONE', #15836, #14096, #1631, .T. ) ;
#9154 = CARTESIAN_POINT ( 'NONE',  ( -13.45468554360235203, -22.38394619046619383, -17.32050807568878170 ) ) ;
#9155 = LINE ( 'NONE', #14926, #9352 ) ;
#9156 = EDGE_CURVE ( 'NONE', #16919, #11811, #9798, .T. ) ;
#9157 = ORIENTED_EDGE ( 'NONE', *, *, #8271, .T. ) ;
#9158 = CIRCLE ( 'NONE', #12939, 12.74754878398196567 ) ;
#9159 = DIRECTION ( 'NONE',  ( -0.1566598588826321192, 0.9876526153536342445, 7.798540720466731404E-17 ) ) ;
#9160 = CYLINDRICAL_SURFACE ( 'NONE', #11083, 1.500000000000001554 ) ;
#9161 = CARTESIAN_POINT ( 'NONE',  ( -51.43967622453926936, -86.11453219379563961, 4.330127018922213189 ) ) ;
#9162 = VERTEX_POINT ( 'NONE', #7304 ) ;
#9163 = ORIENTED_EDGE ( 'NONE', *, *, #4777, .F. ) ;
#9164 = AXIS2_PLACEMENT_3D ( 'NONE', #11634, #2848, #8640 ) ;
#9165 = DIRECTION ( 'NONE',  ( -0.9876526153536336894, -0.1566598588826350336, 0.000000000000000000 ) ) ;
#9166 = AXIS2_PLACEMENT_3D ( 'NONE', #15853, #14431, #13000 ) ;
#9167 = ORIENTED_EDGE ( 'NONE', *, *, #7441, .F. ) ;
#9168 = EDGE_LOOP ( 'NONE', ( #8032, #229, #9627, #3991 ) ) ;
#9169 = ORIENTED_EDGE ( 'NONE', *, *, #199, .T. ) ;
#9170 = CARTESIAN_POINT ( 'NONE',  ( -131.1055737289773617, -2.850701963179328668, 9.951701414186818625E-16 ) ) ;
#9171 = ADVANCED_FACE ( 'NONE', ( #10115 ), #4344, .F. ) ;
#9172 = CARTESIAN_POINT ( 'NONE',  ( -68.72359699322777260, -88.85607972424169532, 8.660254037844412167 ) ) ;
#9173 = CIRCLE ( 'NONE', #11279, 1.500000000000000888 ) ;
#9174 = CARTESIAN_POINT ( 'NONE',  ( -14.40270314877813895, -80.23978748569695085, 8.660254037844412167 ) ) ;
#9175 = DIRECTION ( 'NONE',  ( -0.1566598588826321747, 0.9876526153536343555, 0.000000000000000000 ) ) ;
#9176 = CARTESIAN_POINT ( 'NONE',  ( -8.516422466834198346, -21.60064689605303911, 17.32050807568881012 ) ) ;
#9177 = CARTESIAN_POINT ( 'NONE',  ( -77.18258565727082043, 4.450738551673800281, 20.00000000000000711 ) ) ;
#9178 = ORIENTED_EDGE ( 'NONE', *, *, #10062, .T. ) ;
#9179 = DIRECTION ( 'NONE',  ( -0.1566598588826321192, 0.9876526153536342445, 7.798540720466730171E-17 ) ) ;
#9180 = ORIENTED_EDGE ( 'NONE', *, *, #1740, .T. ) ;
#9181 = CARTESIAN_POINT ( 'NONE',  ( -29.25712738926043244, -24.89050393258829175, 21.65063509461101887 ) ) ;
#9182 = CARTESIAN_POINT ( 'NONE',  ( -23.29157668696081629, -81.64972621564062649, -21.65063509461098690 ) ) ;
#9184 = VERTEX_POINT ( 'NONE', #4046 ) ;
#9183 = CARTESIAN_POINT ( 'NONE',  ( -70.00000000000001421, -45.00000000000001421, 20.00000000000001776 ) ) ;
#9185 = DIRECTION ( 'NONE',  ( -0.000000000000000000, -0.000000000000000000, -1.000000000000000000 ) ) ;
#9186 = AXIS2_PLACEMENT_3D ( 'NONE', #8426, #5592, #14206 ) ;
#9187 = DIRECTION ( 'NONE',  ( -0.1566598588826321192, 0.9876526153536342445, 7.798540720466730171E-17 ) ) ;
#9188 = VERTEX_POINT ( 'NONE', #7388 ) ;
#9189 = ORIENTED_EDGE ( 'NONE', *, *, #14593, .F. ) ;
#9190 = DIRECTION ( 'NONE',  ( -0.1566598588826321192, 0.9876526153536342445, 7.798540720466730171E-17 ) ) ;
#9191 = APPLICATION_CONTEXT ( 'automotive_design' ) ;
#9192 = CARTESIAN_POINT ( 'NONE',  ( -0.1213752363283457369, -20.26903809555066616, -17.32050807568878170 ) ) ;
#9193 = VERTEX_POINT ( 'NONE', #11431 ) ;
#9194 = CARTESIAN_POINT ( 'NONE',  ( 0.4120860815263194254, -77.88988960245745830, -17.32050807568878525 ) ) ;
#9195 = DIRECTION ( 'NONE',  ( -0.1566598588826321747, 0.9876526153536343555, 0.000000000000000000 ) ) ;
#9196 = DIRECTION ( 'NONE',  ( -0.1566598588826321192, 0.9876526153536342445, 7.798540720466731404E-17 ) ) ;
#9197 = CARTESIAN_POINT ( 'NONE',  ( -38.92930022185625205, -21.36217958576385811, 17.32050807568882078 ) ) ;
#9198 = CARTESIAN_POINT ( 'NONE',  ( -47.98289207080156160, -85.56622268770642847, 4.330127018922213189 ) ) ;
#9199 = CARTESIAN_POINT ( 'NONE',  ( -90.00000000000000000, 34.99999999999999289, 30.00000000000002487 ) ) ;
#9200 = CARTESIAN_POINT ( 'NONE',  ( -14.40270314877813895, -80.23978748569693664, -17.32050807568878525 ) ) ;
#9201 = VERTEX_POINT ( 'NONE', #1423 ) ;
#9202 = EDGE_CURVE ( 'NONE', #6188, #10331, #11616, .T. ) ;
#9203 = EDGE_CURVE ( 'NONE', #2224, #7658, #18310, .T. ) ;
#9204 = DIRECTION ( 'NONE',  ( 0.000000000000000000, 1.000000000000000000, 1.224646799147353207E-16 ) ) ;
#9205 = EDGE_LOOP ( 'NONE', ( #16180, #17720, #17148, #763 ) ) ;
#9206 = FACE_OUTER_BOUND ( 'NONE', #4215, .T. ) ;
#9207 = DIRECTION ( 'NONE',  ( -0.1566598588826321192, 0.9876526153536342445, 7.798540720466730171E-17 ) ) ;
#9208 = EDGE_CURVE ( 'NONE', #8349, #10706, #3124, .T. ) ;
#9209 = ORIENTED_EDGE ( 'NONE', *, *, #4393, .T. ) ;
#9210 = VERTEX_POINT ( 'NONE', #2905 ) ;
#9211 = VERTEX_POINT ( 'NONE', #8704 ) ;
#9212 = CARTESIAN_POINT ( 'NONE',  ( -31.68662391746665463, -82.98133501614299234, -4.330127018922185655 ) ) ;
#9213 = EDGE_LOOP ( 'NONE', ( #665, #15147, #15100, #10859 ) ) ;
#9214 = FACE_BOUND ( 'NONE', #17041, .T. ) ;
#9215 = FACE_OUTER_BOUND ( 'NONE', #15630, .T. ) ;
#9216 = ORIENTED_EDGE ( 'NONE', *, *, #14755, .F. ) ;
#9217 = DIRECTION ( 'NONE',  ( 0.000000000000000000, 0.000000000000000000, 1.000000000000000000 ) ) ;
#9218 = DIRECTION ( 'NONE',  ( -0.1566598588826321747, 0.9876526153536343555, 0.000000000000000000 ) ) ;
#9219 = CARTESIAN_POINT ( 'NONE',  ( -26.74836084069850983, -82.19803572172985184, -4.330127018922185655 ) ) ;
#9220 = DIRECTION ( 'NONE',  ( 0.9868632313631133801, -0.1615579233078772714, 0.000000000000000000 ) ) ;
#9221 = VERTEX_POINT ( 'NONE', #5685 ) ;
#9222 = ORIENTED_EDGE ( 'NONE', *, *, #13123, .F. ) ;
#9223 = DIRECTION ( 'NONE',  ( 1.000000000000000000, 0.000000000000000000, 0.000000000000000000 ) ) ;
#9224 = EDGE_CURVE ( 'NONE', #12364, #3748, #15997, .T. ) ;
#9225 = AXIS2_PLACEMENT_3D ( 'NONE', #13367, #11916, #7780 ) ;
#9226 = DIRECTION ( 'NONE',  ( -0.1566598588826321192, 0.9876526153536342445, 7.798540720466731404E-17 ) ) ;
#9227 = ORIENTED_EDGE ( 'NONE', *, *, #13764, .T. ) ;
#9228 = DIRECTION ( 'NONE',  ( -0.1566598588826321192, 0.9876526153536342445, 7.798540720466730171E-17 ) ) ;
#9229 = EDGE_CURVE ( 'NONE', #17343, #6767, #17440, .T. ) ;
#9230 = ORIENTED_EDGE ( 'NONE', *, *, #4906, .T. ) ;
#9231 = DIRECTION ( 'NONE',  ( -0.000000000000000000, -0.000000000000000000, -1.000000000000000000 ) ) ;
#9232 = AXIS2_PLACEMENT_3D ( 'NONE', #8099, #9625, #14063 ) ;
#9233 = DIRECTION ( 'NONE',  ( -0.1566598588826321192, 0.9876526153536342445, 7.798540720466731404E-17 ) ) ;
#9234 = EDGE_LOOP ( 'NONE', ( #9528, #13158, #11750, #5536 ) ) ;
#9235 = CARTESIAN_POINT ( 'NONE',  ( -36.66452200441266029, -26.06545287420802737, -17.32050807568878170 ) ) ;
#9236 = SURFACE_STYLE_USAGE ( .BOTH. , #1857 ) ;
#9237 = DIRECTION ( 'NONE',  ( -0.1566598588826321192, 0.9876526153536342445, 7.798540720466730171E-17 ) ) ;
#9238 = EDGE_LOOP ( 'NONE', ( #16145, #9661 ) ) ;
#9239 = VERTEX_POINT ( 'NONE', #12951 ) ;
#9240 = DIRECTION ( 'NONE',  ( -0.1566598588826321192, 0.9876526153536342445, 7.798540720466730171E-17 ) ) ;
#9241 = EDGE_CURVE ( 'NONE', #3908, #12253, #5500, .T. ) ;
#9242 = ORIENTED_EDGE ( 'NONE', *, *, #8423, .T. ) ;
#9243 = ORIENTED_EDGE ( 'NONE', *, *, #14100, .F. ) ;
#9244 = ADVANCED_FACE ( 'NONE', ( #14484 ), #13054, .T. ) ;
#9245 = EDGE_LOOP ( 'NONE', ( #16704, #13961, #15649, #15577 ) ) ;
#9246 = VECTOR ( 'NONE', #616, 1000.000000000000000 ) ;
#9247 = EDGE_LOOP ( 'NONE', ( #17639, #10975, #3404, #8929 ) ) ;
#9248 = ADVANCED_FACE ( 'NONE', ( #12865 ), #4250, .F. ) ;
#9249 = VERTEX_POINT ( 'NONE', #14581 ) ;
#9250 = CARTESIAN_POINT ( 'NONE',  ( -2.879979761448749009, -15.64409473654778893, 1.579620830366336657E-14 ) ) ;
#9251 = CARTESIAN_POINT ( 'NONE',  ( -65.30644784966793281, -30.60858878180435738, 4.330127018922217630 ) ) ;
#9252 = ORIENTED_EDGE ( 'NONE', *, *, #17170, .F. ) ;
#9253 = CARTESIAN_POINT ( 'NONE',  ( -4.565812005419673802, -20.97400746052251108, -21.65063509461098334 ) ) ;
#9254 = AXIS2_PLACEMENT_3D ( 'NONE', #12964, #8545, #14320 ) ;
#9255 = CARTESIAN_POINT ( 'NONE',  ( 73.09088021254186174, 1.387778780781445676E-14, 25.00000000000000000 ) ) ;
#9256 = DIRECTION ( 'NONE',  ( 0.1856185419698760941, -0.9826218788918640312, 0.000000000000000000 ) ) ;
#9257 = CARTESIAN_POINT ( 'NONE',  ( 1.399738696879940791, -77.73322974357483872, -21.65063509461098690 ) ) ;
#9258 = CIRCLE ( 'NONE', #3183, 1.499999999999999556 ) ;
#9259 = CARTESIAN_POINT ( 'NONE',  ( -129.1404785418517918, -2.850701963179328668, -15.74754878398195856 ) ) ;
#9260 = FACE_OUTER_BOUND ( 'NONE', #11120, .T. ) ;
#9261 = CARTESIAN_POINT ( 'NONE',  ( -70.00000000000000000, 44.99999999999999289, 7.500000000000007105 ) ) ;
#9262 = ADVANCED_FACE ( 'NONE', ( #2638 ), #4141, .T. ) ;
#9264 = ORIENTED_EDGE ( 'NONE', *, *, #7442, .F. ) ;
#9263 = DIRECTION ( 'NONE',  ( -0.1566598588826321747, 0.9876526153536343555, 0.000000000000000000 ) ) ;
#9265 = EDGE_CURVE ( 'NONE', #2699, #10382, #9496, .T. ) ;
#9266 = DIRECTION ( 'NONE',  ( -0.000000000000000000, -0.000000000000000000, -1.000000000000000000 ) ) ;
#9267 = EDGE_CURVE ( 'NONE', #12882, #13318, #1247, .T. ) ;
#9268 = DIRECTION ( 'NONE',  ( -0.000000000000000000, -0.000000000000000000, -1.000000000000000000 ) ) ;
#9269 = ORIENTED_EDGE ( 'NONE', *, *, #16212, .F. ) ;
#9270 = EDGE_LOOP ( 'NONE', ( #4079, #18147 ) ) ;
#9271 = VERTEX_POINT ( 'NONE', #18625 ) ;
#9272 = CIRCLE ( 'NONE', #14728, 1.500000000000000444 ) ;
#9273 = CARTESIAN_POINT ( 'NONE',  ( -62.83731631128384976, -30.21693913459777647, 17.32050807568881723 ) ) ;
#9274 = EDGE_LOOP ( 'NONE', ( #17022, #3912 ) ) ;
#9275 = DIRECTION ( 'NONE',  ( -0.9876526153536341335, -0.1566598588826327021, 0.000000000000000000 ) ) ;
#9276 = CARTESIAN_POINT ( 'NONE',  ( -34.97868976044174616, -20.73554015023331942, -21.65063509461098334 ) ) ;
#9277 = FACE_OUTER_BOUND ( 'NONE', #8782, .T. ) ;
#9278 = UNCERTAINTY_MEASURE_WITH_UNIT (LENGTH_MEASURE( 1.000000000000000082E-05 ), #681, 'distance_accuracy_value', 'NONE');
#9279 = AXIS2_PLACEMENT_3D ( 'NONE', #3535, #13485, #17909 ) ;
#9280 = CARTESIAN_POINT ( 'NONE',  ( -127.5081579206795936, -15.25292806682357494, -2.822349119005437057 ) ) ;
#9281 = DIRECTION ( 'NONE',  ( 0.9876526153536341335, -0.1566598588826326743, 0.000000000000000000 ) ) ;
#9282 = CARTESIAN_POINT ( 'NONE',  ( 2.000000000000000000, 0.000000000000000000, 35.00000000000000000 ) ) ;
#9283 = DIRECTION ( 'NONE',  ( -0.000000000000000000, -0.000000000000000000, -1.000000000000000000 ) ) ;
#9284 = ORIENTED_EDGE ( 'NONE', *, *, #6966, .T. ) ;
#9285 = PRESENTATION_STYLE_ASSIGNMENT (( #3489 ) ) ;
#9286 = CARTESIAN_POINT ( 'NONE',  ( -77.65210554158829837, -32.56683701783724416, -8.660254037844380193 ) ) ;
#9287 = COLOUR_RGB ( '', 0.66274510, 0.83137255, 0.94901961) ;
#9288 = VECTOR ( 'NONE', #17558, 1000.000000000000000 ) ;
#9289 = LINE ( 'NONE', #2186, #8159 ) ;
#9290 = ORIENTED_EDGE ( 'NONE', *, *, #8245, .F. ) ;
#9291 = ORIENTED_EDGE ( 'NONE', *, *, #8676, .F. ) ;
#9292 = ORIENTED_EDGE ( 'NONE', *, *, #5420, .T. ) ;
#9293 = ORIENTED_EDGE ( 'NONE', *, *, #11202, .F. ) ;
#9294 = CARTESIAN_POINT ( 'NONE',  ( -13.41505053342451426, -80.08312762681431707, -12.99038105676658539 ) ) ;
#9295 = AXIS2_PLACEMENT_3D ( 'NONE', #14723, #8760, #10088 ) ;
#9296 = FACE_BOUND ( 'NONE', #14895, .T. ) ;
#9297 = EDGE_CURVE ( 'NONE', #15897, #17878, #11342, .T. ) ;
#9298 = EDGE_CURVE ( 'NONE', #13520, #6246, #15842, .T. ) ;
#9299 = DIRECTION ( 'NONE',  ( -0.1566598588826321192, 0.9876526153536342445, 7.798540720466731404E-17 ) ) ;
#9300 = CYLINDRICAL_SURFACE ( 'NONE', #1892, 1.500000000000000666 ) ;
#9301 =( GEOMETRIC_REPRESENTATION_CONTEXT ( 3 ) GLOBAL_UNCERTAINTY_ASSIGNED_CONTEXT ( ( #11907 ) ) GLOBAL_UNIT_ASSIGNED_CONTEXT ( ( #13122, #12930, #2886 ) ) REPRESENTATION_CONTEXT ( 'NONE', 'WORKASPACE' ) );
#9302 = CIRCLE ( 'NONE', #11412, 1.500000000000000888 ) ;
#9303 = AXIS2_PLACEMENT_3D ( 'NONE', #143, #4401, #2968 ) ;
#9304 = EDGE_LOOP ( 'NONE', ( #17488, #11030, #4778, #11414 ) ) ;
#9305 = LINE ( 'NONE', #8936, #14235 ) ;
#9306 = CARTESIAN_POINT ( 'NONE',  ( -63.62061560569701157, -25.27867605782963878, -8.660254037844380193 ) ) ;
#9307 = CARTESIAN_POINT ( 'NONE',  ( -7.034943543803747090, -21.36565710772908488, 17.32050807568881012 ) ) ;
#9308 = PLANE ( 'NONE',  #12562 ) ;
#9309 = CARTESIAN_POINT ( 'NONE',  ( -129.1404785418517918, -15.35070196317932911, 2.500000000000000000 ) ) ;
#9310 = EDGE_LOOP ( 'NONE', ( #13626, #15940, #2176, #2624 ) ) ;
#9311 = ORIENTED_EDGE ( 'NONE', *, *, #7468, .F. ) ;
#9312 = DIRECTION ( 'NONE',  ( -0.1566598588826321192, 0.9876526153536342445, 7.798540720466730171E-17 ) ) ;
#9313 = CARTESIAN_POINT ( 'NONE',  ( -35.63723437888119605, -83.60797445167352748, -8.660254037844385522 ) ) ;
#9314 = CARTESIAN_POINT ( 'NONE',  ( -64.20000000000000284, 2.694222958124175527E-16, 20.00000000000001776 ) ) ;
#9315 = DIRECTION ( 'NONE',  ( -0.1566598588826321192, 0.9876526153536342445, 7.798540720466730171E-17 ) ) ;
#9316 = ORIENTED_EDGE ( 'NONE', *, *, #16826, .F. ) ;
#9317 = ORIENTED_EDGE ( 'NONE', *, *, #270, .T. ) ;
#9318 = DIRECTION ( 'NONE',  ( -0.1566598588826321470, 0.9876526153536342445, 0.000000000000000000 ) ) ;
#9319 = ADVANCED_FACE ( 'NONE', ( #7469, #171 ), #10581, .F. ) ;
#9320 = EDGE_LOOP ( 'NONE', ( #10989, #1917, #13592, #2849 ) ) ;
#9321 = CIRCLE ( 'NONE', #6928, 1.500000000000000888 ) ;
#9322 = VECTOR ( 'NONE', #6492, 1000.000000000000000 ) ;
#9323 = FACE_OUTER_BOUND ( 'NONE', #2316, .T. ) ;
#9324 = AXIS2_PLACEMENT_3D ( 'NONE', #10697, #6466, #12199 ) ;
#9325 = AXIS2_PLACEMENT_3D ( 'NONE', #3808, #11113, #8098 ) ;
#9326 = ADVANCED_FACE ( 'NONE', ( #8890 ), #13330, .F. ) ;
#9327 = LINE ( 'NONE', #11870, #13898 ) ;
#9328 = DIRECTION ( 'NONE',  ( -0.1566598588826321192, 0.9876526153536342445, 7.798540720466731404E-17 ) ) ;
#9329 = ORIENTED_EDGE ( 'NONE', *, *, #11598, .T. ) ;
#9330 = CYLINDRICAL_SURFACE ( 'NONE', #292, 1.500000000000001554 ) ;
#9331 = DIRECTION ( 'NONE',  ( -0.1566598588826321192, 0.9876526153536342445, 7.798540720466730171E-17 ) ) ;
#9332 = CARTESIAN_POINT ( 'NONE',  ( -72.71384246482016067, -31.78353772342409300, 17.32050807568881723 ) ) ;
#9333 = ORIENTED_EDGE ( 'NONE', *, *, #8386, .F. ) ;
#9334 = ORIENTED_EDGE ( 'NONE', *, *, #8386, .T. ) ;
#9335 = CYLINDRICAL_SURFACE ( 'NONE', #8197, 1.500000000000001554 ) ;
#9336 = CIRCLE ( 'NONE', #17853, 5.000000000000000000 ) ;
#9337 = ORIENTED_EDGE ( 'NONE', *, *, #1770, .T. ) ;
#9338 = ORIENTED_EDGE ( 'NONE', *, *, #3122, .T. ) ;
#9339 = AXIS2_PLACEMENT_3D ( 'NONE', #11975, #2057, #3654 ) ;
#9340 = AXIS2_PLACEMENT_3D ( 'NONE', #9219, #15000, #9031 ) ;
#9341 = VERTEX_POINT ( 'NONE', #17539 ) ;
#9342 = ORIENTED_EDGE ( 'NONE', *, *, #7118, .T. ) ;
#9343 = CARTESIAN_POINT ( 'NONE',  ( -56.41757431148526081, -29.19865005186066753, -8.660254037844380193 ) ) ;
#9344 = VECTOR ( 'NONE', #13441, 1000.000000000000000 ) ;
#9345 = CARTESIAN_POINT ( 'NONE',  ( -20.86208015875458344, -23.55889513208593655, 12.99038105676661736 ) ) ;
#9346 = DIRECTION ( 'NONE',  ( 1.000000000000000000, 0.000000000000000000, 0.000000000000000000 ) ) ;
#9347 = EDGE_LOOP ( 'NONE', ( #9599, #2674, #8372, #9556 ) ) ;
#9348 = ADVANCED_FACE ( 'NONE', ( #14668 ), #3456, .T. ) ;
#9349 = CARTESIAN_POINT ( 'NONE',  ( -1.109027851681966492, -20.42569795443330349, 21.65063509461101177 ) ) ;
#9350 = LINE ( 'NONE', #3272, #10350 ) ;
#9351 = AXIS2_PLACEMENT_3D ( 'NONE', #11681, #14737, #4327 ) ;
#9352 = VECTOR ( 'NONE', #343, 1000.000000000000000 ) ;
#9353 = DIRECTION ( 'NONE',  ( -0.1566598588826321747, 0.9876526153536343555, 0.000000000000000000 ) ) ;
#9354 = CIRCLE ( 'NONE', #6640, 15.83618137761393463 ) ;
#9355 = CYLINDRICAL_SURFACE ( 'NONE', #17179, 1.500000000000000888 ) ;
#9356 = FACE_BOUND ( 'NONE', #13476, .T. ) ;
#9357 = ADVANCED_FACE ( 'NONE', ( #17925 ), #6343, .F. ) ;
#9358 = DIRECTION ( 'NONE',  ( -0.1566598588826321192, 0.9876526153536342445, 7.798540720466730171E-17 ) ) ;
#9359 = DIRECTION ( 'NONE',  ( -0.1566598588826321192, 0.9876526153536342445, 7.798540720466731404E-17 ) ) ;
#9360 = CYLINDRICAL_SURFACE ( 'NONE', #4145, 1.500000000000000666 ) ;
#9362 = ORIENTED_EDGE ( 'NONE', *, *, #7889, .T. ) ;
#9361 = DIRECTION ( 'NONE',  ( 0.000000000000000000, 0.000000000000000000, 1.000000000000000000 ) ) ;
#9363 = AXIS2_PLACEMENT_3D ( 'NONE', #6101, #4656, #1725 ) ;
#9364 = DIRECTION ( 'NONE',  ( -0.1566598588826321747, 0.9876526153536343555, 0.000000000000000000 ) ) ;
#9365 = ORIENTED_EDGE ( 'NONE', *, *, #1767, .T. ) ;
#9366 = AXIS2_PLACEMENT_3D ( 'NONE', #9774, #6945, #2655 ) ;
#9367 = EDGE_LOOP ( 'NONE', ( #3993, #13687, #16979, #6561 ) ) ;
#9368 = VERTEX_POINT ( 'NONE', #1873 ) ;
#9369 = CIRCLE ( 'NONE', #1528, 1.500000000000000888 ) ;
#9370 = CIRCLE ( 'NONE', #13283, 1.500000000000001332 ) ;
#9371 = EDGE_CURVE ( 'NONE', #9146, #18003, #8289, .T. ) ;
#9372 = CARTESIAN_POINT ( 'NONE',  ( -28.06512145296634486, -19.63892113805490069, -4.330127018922180326 ) ) ;
#9373 = CARTESIAN_POINT ( 'NONE',  ( -9.464440072009985272, -79.45648819128378193, -8.660254037844385522 ) ) ;
#9374 = DIRECTION ( 'NONE',  ( 0.000000000000000000, 0.000000000000000000, 1.000000000000000000 ) ) ;
#9375 = AXIS2_PLACEMENT_3D ( 'NONE', #1427, #3181, #4618 ) ;
#9376 = EDGE_CURVE ( 'NONE', #8333, #4400, #7384, .T. ) ;
#9377 = CARTESIAN_POINT ( 'NONE',  ( -127.6870874808773664, -15.23343154280193978, -2.921574671186279559 ) ) ;
#9378 = EDGE_CURVE ( 'NONE', #8719, #10299, #7976, .T. ) ;
#9379 = DIRECTION ( 'NONE',  ( -0.000000000000000000, -0.000000000000000000, -1.000000000000000000 ) ) ;
#9380 = CARTESIAN_POINT ( 'NONE',  ( 9.300959619708997650, -76.47995087251376845, -21.65063509461098690 ) ) ;
#9381 = AXIS2_PLACEMENT_3D ( 'NONE', #18585, #7083, #17121 ) ;
#9382 = DIRECTION ( 'NONE',  ( -0.1566598588826321192, 0.9876526153536342445, 7.798540720466730171E-17 ) ) ;
#9383 = EDGE_LOOP ( 'NONE', ( #14714, #16583 ) ) ;
#9384 = DIRECTION ( 'NONE',  ( -0.1566598588826321192, 0.9876526153536342445, 7.798540720466731404E-17 ) ) ;
#9385 = ORIENTED_EDGE ( 'NONE', *, *, #9265, .T. ) ;
#9386 = FACE_BOUND ( 'NONE', #9942, .T. ) ;
#9387 = EDGE_CURVE ( 'NONE', #13932, #9656, #17083, .T. ) ;
#9388 = VECTOR ( 'NONE', #10355, 1000.000000000000114 ) ;
#9389 = DIRECTION ( 'NONE',  ( -0.9876526153536341335, -0.1566598588826327021, 0.000000000000000000 ) ) ;
#9390 = LINE ( 'NONE', #6749, #912 ) ;
#9391 = CARTESIAN_POINT ( 'NONE',  ( -53.94844277310116354, -28.80700040465408662, 21.65063509461101887 ) ) ;
#9392 = VECTOR ( 'NONE', #10698, 1000.000000000000000 ) ;
#9393 = EDGE_CURVE ( 'NONE', #5203, #9088, #3178, .T. ) ;
#9394 = ORIENTED_EDGE ( 'NONE', *, *, #13623, .T. ) ;
#9395 = DIRECTION ( 'NONE',  ( 0.000000000000000000, 0.000000000000000000, 1.000000000000000000 ) ) ;
#9396 = EDGE_LOOP ( 'NONE', ( #11695, #565 ) ) ;
#9397 = VERTEX_POINT ( 'NONE', #13232 ) ;
#9398 = CIRCLE ( 'NONE', #3316, 1.500000000000000444 ) ;
#9399 = EDGE_LOOP ( 'NONE', ( #18572, #5430 ) ) ;
#9400 = DIRECTION ( 'NONE',  ( -0.1566598588826321192, 0.9876526153536342445, 7.798540720466731404E-17 ) ) ;
#9401 = VECTOR ( 'NONE', #16972, 1000.000000000000000 ) ;
#9402 = FACE_BOUND ( 'NONE', #4108, .T. ) ;
#9403 = VECTOR ( 'NONE', #116, 1000.000000000000227 ) ;
#9404 = CARTESIAN_POINT ( 'NONE',  ( 5.005906274354423851E-15, -2.200000000000007283, 20.00000000000000000 ) ) ;
#9405 = CIRCLE ( 'NONE', #4846, 1.500000000000000888 ) ;
#9406 = AXIS2_PLACEMENT_3D ( 'NONE', #11407, #15797, #17052 ) ;
#9407 = ADVANCED_FACE ( 'NONE', ( #3270 ), #6154, .F. ) ;
#9408 = EDGE_CURVE ( 'NONE', #1267, #9967, #10384, .T. ) ;
#9409 = DIRECTION ( 'NONE',  ( 0.000000000000000000, 0.000000000000000000, 1.000000000000000000 ) ) ;
#9410 = AXIS2_PLACEMENT_3D ( 'NONE', #3649, #16562, #8220 ) ;
#9411 = ADVANCED_FACE ( 'NONE', ( #9074 ), #12075, .F. ) ;
#9412 = PLANE ( 'NONE',  #3322 ) ;
#9413 = CARTESIAN_POINT ( 'NONE',  ( 4.362696542940843081, -77.26325016692693737, 4.330127018922209636 ) ) ;
#9414 = PRODUCT_DEFINITION ( 'UNKNOWN', '', #10218, #11298 ) ;
#9415 = ADVANCED_FACE ( 'NONE', ( #7743 ), #14851, .F. ) ;
#9416 = DIRECTION ( 'NONE',  ( -0.9876526153536341335, -0.1566598588826327021, 0.000000000000000000 ) ) ;
#9417 = ORIENTED_EDGE ( 'NONE', *, *, #11966, .F. ) ;
#9418 = ORIENTED_EDGE ( 'NONE', *, *, #7425, .F. ) ;
#9419 = CARTESIAN_POINT ( 'NONE',  ( -21.81009776393036503, -81.41473642731668292, 4.330127018922213189 ) ) ;
#9420 = DIRECTION ( 'NONE',  ( -0.1566598588826321192, 0.9876526153536342445, 7.798540720466731404E-17 ) ) ;
#9421 = AXIS2_PLACEMENT_3D ( 'NONE', #3617, #13394, #6217 ) ;
#9422 = ORIENTED_EDGE ( 'NONE', *, *, #1524, .T. ) ;
#9423 = DIRECTION ( 'NONE',  ( -0.1566598588826321747, 0.9876526153536343555, 0.000000000000000000 ) ) ;
#9424 = ORIENTED_EDGE ( 'NONE', *, *, #3668, .F. ) ;
#9425 = DIRECTION ( 'NONE',  ( -0.1566598588826321747, 0.9876526153536343555, 0.000000000000000000 ) ) ;
#9426 = AXIS2_PLACEMENT_3D ( 'NONE', #2073, #3669, #10965 ) ;
#9427 = VECTOR ( 'NONE', #1017, 1000.000000000000000 ) ;
#9428 = CYLINDRICAL_SURFACE ( 'NONE', #7590, 1.500000000000001554 ) ;
#9429 = CIRCLE ( 'NONE', #1284, 1.500000000000000888 ) ;
#9430 = CARTESIAN_POINT ( 'NONE',  ( -70.00000000000002842, 45.00000000000000000, 20.00000000000001776 ) ) ;
#9431 = FACE_OUTER_BOUND ( 'NONE', #7105, .T. ) ;
#9432 = SURFACE_STYLE_USAGE ( .BOTH. , #5166 ) ;
#9433 = DIRECTION ( 'NONE',  ( 0.000000000000000000, 0.000000000000000000, 1.000000000000000000 ) ) ;
#9434 = FILL_AREA_STYLE_COLOUR ( '', #9287 ) ;
#9435 = EDGE_CURVE ( 'NONE', #1456, #11968, #5252, .T. ) ;
#9436 = CIRCLE ( 'NONE', #10330, 1.500000000000000888 ) ;
#9437 = CARTESIAN_POINT ( 'NONE',  ( -46.33669483700850122, -22.53712852738357952, -21.65063509461097979 ) ) ;
#9438 = EDGE_LOOP ( 'NONE', ( #14254, #14295 ) ) ;
#9439 = EDGE_CURVE ( 'NONE', #3971, #4926, #10085, .T. ) ;
#9440 = ORIENTED_EDGE ( 'NONE', *, *, #3902, .F. ) ;
#9441 = APPLICATION_CONTEXT ( 'automotive_design' ) ;
#9442 = CARTESIAN_POINT ( 'NONE',  ( -50.49165861936349131, -28.25869089856488614, -12.99038105676658006 ) ) ;
#9443 = EDGE_LOOP ( 'NONE', ( #9064, #3549 ) ) ;
#9444 = VECTOR ( 'NONE', #1777, 1000.000000000000000 ) ;
#9445 = ADVANCED_FACE ( 'NONE', ( #4700 ), #3413, .T. ) ;
#9446 = DIRECTION ( 'NONE',  ( -0.1566598588826321747, 0.9876526153536343555, 0.000000000000000000 ) ) ;
#9447 = EDGE_LOOP ( 'NONE', ( #298, #15458, #11152, #4985 ) ) ;
#9448 = VERTEX_POINT ( 'NONE', #9643 ) ;
#9449 = VECTOR ( 'NONE', #10606, 1000.000000000000000 ) ;
#9450 = DIRECTION ( 'NONE',  ( -0.9876526153536341335, -0.1566598588826327021, 0.000000000000000000 ) ) ;
#9451 = AXIS2_PLACEMENT_3D ( 'NONE', #13259, #10141, #293 ) ;
#9452 = CARTESIAN_POINT ( 'NONE',  ( -18.18859529943003750, -18.07232254922858417, -4.330127018922180326 ) ) ;
#9453 = CARTESIAN_POINT ( 'NONE',  ( -79.13358446461874962, -32.80182680616118773, 8.660254037844417496 ) ) ;
#9454 = DIRECTION ( 'NONE',  ( -3.208277787129350839E-17, -0.000000000000000000, 1.000000000000000000 ) ) ;
#9455 = VECTOR ( 'NONE', #9698, 1000.000000000000000 ) ;
#9456 = CARTESIAN_POINT ( 'NONE',  ( -15.71946376104596155, -17.68067290202200326, 17.32050807568881012 ) ) ;
#9457 = CYLINDRICAL_SURFACE ( 'NONE', #13787, 1.500000000000001554 ) ;
#9458 = LINE ( 'NONE', #15230, #4164 ) ;
#9459 = CARTESIAN_POINT ( 'NONE',  ( -48.80582637539254875, -22.92877817459017464, 17.32050807568882078 ) ) ;
#9461 = VERTEX_POINT ( 'NONE', #15317 ) ;
#9460 = DIRECTION ( 'NONE',  ( -0.1566598588826321192, 0.9876526153536342445, 7.798540720466730171E-17 ) ) ;
#9462 = ORIENTED_EDGE ( 'NONE', *, *, #2145, .F. ) ;
#9463 = DIRECTION ( 'NONE',  ( -0.1566598588826321192, 0.9876526153536342445, 7.798540720466730171E-17 ) ) ;
#9464 = EDGE_CURVE ( 'NONE', #16710, #17960, #9749, .T. ) ;
#9465 = ORIENTED_EDGE ( 'NONE', *, *, #9575, .F. ) ;
#9466 = ORIENTED_EDGE ( 'NONE', *, *, #3564, .T. ) ;
#9467 = VECTOR ( 'NONE', #9668, 1000.000000000000000 ) ;
#9468 = FACE_OUTER_BOUND ( 'NONE', #18143, .T. ) ;
#9469 = ADVANCED_FACE ( 'NONE', ( #18312 ), #10750, .F. ) ;
#9470 = ORIENTED_EDGE ( 'NONE', *, *, #16946, .F. ) ;
#9471 = ORIENTED_EDGE ( 'NONE', *, *, #7495, .T. ) ;
#9472 = DIRECTION ( 'NONE',  ( -0.1566598588826321747, 0.9876526153536343555, 0.000000000000000000 ) ) ;
#9473 = ORIENTED_EDGE ( 'NONE', *, *, #15531, .T. ) ;
#9474 = DIRECTION ( 'NONE',  ( -0.9876526153536341335, -0.1566598588826327021, 0.000000000000000000 ) ) ;
#9475 = DIRECTION ( 'NONE',  ( 1.000000000000000000, 0.000000000000000000, -0.000000000000000000 ) ) ;
#9476 = CARTESIAN_POINT ( 'NONE',  ( -26.58364252993588650, -19.40393134973096068, 21.65063509461102242 ) ) ;
#9477 = CARTESIAN_POINT ( 'NONE',  ( 2.200000000000000178, 2.694222958124177006E-16, -19.99999999999999645 ) ) ;
#9478 = LINE ( 'NONE', #1070, #7460 ) ;
#9479 = VERTEX_POINT ( 'NONE', #10845 ) ;
#9480 = CARTESIAN_POINT ( 'NONE',  ( 3.231158466157545206, -19.73726462726228092, 35.00000000000000000 ) ) ;
#9481 = AXIS2_PLACEMENT_3D ( 'NONE', #10028, #1608, #8622 ) ;
#9482 = CARTESIAN_POINT ( 'NONE',  ( -62.83731631128384976, -30.21693913459777647, 17.32050807568881723 ) ) ;
#9483 = ORIENTED_EDGE ( 'NONE', *, *, #3150, .T. ) ;
#9484 = FACE_OUTER_BOUND ( 'NONE', #9367, .T. ) ;
#9485 = ORIENTED_EDGE ( 'NONE', *, *, #9030, .T. ) ;
#9486 = ORIENTED_EDGE ( 'NONE', *, *, #13124, .T. ) ;
#9487 = DIRECTION ( 'NONE',  ( -0.1566598588826321192, 0.9876526153536342445, 7.798540720466730171E-17 ) ) ;
#9488 = ORIENTED_EDGE ( 'NONE', *, *, #2307, .T. ) ;
#9489 = ORIENTED_EDGE ( 'NONE', *, *, #1246, .F. ) ;
#9490 = DIRECTION ( 'NONE',  ( 1.000000000000000000, 0.000000000000000000, -0.000000000000000000 ) ) ;
#9491 = EDGE_CURVE ( 'NONE', #1168, #8810, #17688, .T. ) ;
#9492 = EDGE_CURVE ( 'NONE', #6188, #7482, #2838, .T. ) ;
#9493 = VERTEX_POINT ( 'NONE', #11034 ) ;
#9494 = FACE_BOUND ( 'NONE', #17874, .T. ) ;
#9495 = EDGE_CURVE ( 'NONE', #14919, #4926, #15418, .T. ) ;
#9496 = CIRCLE ( 'NONE', #9186, 1.499999999999999556 ) ;
#9497 =( LENGTH_UNIT ( ) NAMED_UNIT ( * ) SI_UNIT ( .MILLI., .METRE. ) );
#9498 = ORIENTED_EDGE ( 'NONE', *, *, #9598, .T. ) ;
#9499 = CARTESIAN_POINT ( 'NONE',  ( -26.74836084069852404, -82.19803572172983763, -21.65063509461098690 ) ) ;
#9500 = FACE_BOUND ( 'NONE', #1880, .T. ) ;
#9501 = DIRECTION ( 'NONE',  ( -0.9876526153536336894, -0.1566598588826349503, 0.000000000000000000 ) ) ;
#9502 = DIRECTION ( 'NONE',  ( -0.1566598588826321192, 0.9876526153536342445, 7.798540720466731404E-17 ) ) ;
#9503 = DIRECTION ( 'NONE',  ( -0.1566598588826321192, 0.9876526153536342445, 7.798540720466731404E-17 ) ) ;
#9504 = DIRECTION ( 'NONE',  ( 0.000000000000000000, 0.000000000000000000, 1.000000000000000000 ) ) ;
#9505 = ORIENTED_EDGE ( 'NONE', *, *, #8295, .F. ) ;
#9506 = ORIENTED_EDGE ( 'NONE', *, *, #9852, .F. ) ;
#9507 = DIRECTION ( 'NONE',  ( 0.000000000000000000, 0.000000000000000000, 1.000000000000000000 ) ) ;
#9508 = DIRECTION ( 'NONE',  ( 0.000000000000000000, 0.000000000000000000, -1.000000000000000000 ) ) ;
#9509 = EDGE_CURVE ( 'NONE', #11897, #17960, #11884, .T. ) ;
#9510 = DIRECTION ( 'NONE',  ( -0.1566598588826321192, 0.9876526153536342445, 7.798540720466730171E-17 ) ) ;
#9511 = EDGE_LOOP ( 'NONE', ( #13619, #11517, #9466, #13166 ) ) ;
#9512 = ORIENTED_EDGE ( 'NONE', *, *, #5345, .F. ) ;
#9513 = VERTEX_POINT ( 'NONE', #16670 ) ;
#9514 = LINE ( 'NONE', #2585, #9120 ) ;
#9515 = EDGE_CURVE ( 'NONE', #16711, #8532, #5261, .T. ) ;
#9516 = ORIENTED_EDGE ( 'NONE', *, *, #3274, .F. ) ;
#9517 = CARTESIAN_POINT ( 'NONE',  ( -19.34096622554629263, -81.02308678011010556, 8.660254037844412167 ) ) ;
#9518 = CARTESIAN_POINT ( 'NONE',  ( -167.8715234159095928, 32.08088783854852011, 2.520603730400378772 ) ) ;
#9519 = CARTESIAN_POINT ( 'NONE',  ( -52.92115514756972061, -86.34952198211959740, 4.330127018922213189 ) ) ;
#9520 = FACE_OUTER_BOUND ( 'NONE', #14827, .T. ) ;
#9521 = CARTESIAN_POINT ( 'NONE',  ( 0.000000000000000000, 0.000000000000000000, 0.000000000000000000 ) ) ;
#9522 = DIRECTION ( 'NONE',  ( -0.1566598588826321192, 0.9876526153536342445, 7.798540720466730171E-17 ) ) ;
#9523 = DIRECTION ( 'NONE',  ( -0.1566598588826321192, 0.9876526153536342445, 7.798540720466731404E-17 ) ) ;
#9524 = CARTESIAN_POINT ( 'NONE',  ( -36.46016868347218320, -20.97052993855727365, 4.330127018922218518 ) ) ;
#9525 = DIRECTION ( 'NONE',  ( 0.000000000000000000, 0.000000000000000000, 1.000000000000000000 ) ) ;
#9526 = CARTESIAN_POINT ( 'NONE',  ( -68.72359699322777260, -88.85607972424168111, 1.424741226644455312E-14 ) ) ;
#9527 = VERTEX_POINT ( 'NONE', #4971 ) ;
#9528 = ORIENTED_EDGE ( 'NONE', *, *, #14034, .F. ) ;
#9529 = DIRECTION ( 'NONE',  ( -0.1566598588826321192, 0.9876526153536342445, 7.798540720466731404E-17 ) ) ;
#9530 = VERTEX_POINT ( 'NONE', #13993 ) ;
#9531 = ORIENTED_EDGE ( 'NONE', *, *, #4297, .F. ) ;
#9532 = DIRECTION ( 'NONE',  ( -0.9876526153536336894, -0.1566598588826350336, 0.000000000000000000 ) ) ;
#9533 = ORIENTED_EDGE ( 'NONE', *, *, #8831, .F. ) ;
#9534 = VERTEX_POINT ( 'NONE', #16564 ) ;
#9535 = CARTESIAN_POINT ( 'NONE',  ( -6.830590222863280658, -16.27073417207831696, 21.65063509461101532 ) ) ;
#9536 = VERTEX_POINT ( 'NONE', #1046 ) ;
#9537 = AXIS2_PLACEMENT_3D ( 'NONE', #11781, #8956, #8878 ) ;
#9538 = DIRECTION ( 'NONE',  ( -0.1566598588826321192, 0.9876526153536342445, 7.798540720466730171E-17 ) ) ;
#9539 = EDGE_CURVE ( 'NONE', #272, #1095, #8020, .T. ) ;
#9540 = ORIENTED_EDGE ( 'NONE', *, *, #4723, .F. ) ;
#9541 = CARTESIAN_POINT ( 'NONE',  ( -72.71384246482016067, -31.78353772342409300, -8.660254037844380193 ) ) ;
#9542 = EDGE_CURVE ( 'NONE', #17453, #16580, #3548, .T. ) ;
#9543 = CARTESIAN_POINT ( 'NONE',  ( -64.60826822105063627, -25.43533591671228322, 12.99038105676661736 ) ) ;
#9544 = ORIENTED_EDGE ( 'NONE', *, *, #3561, .F. ) ;
#9545 = DIRECTION ( 'NONE',  ( -0.1856185419698762329, 0.9826218788918640312, -0.000000000000000000 ) ) ;
#9546 = DIRECTION ( 'NONE',  ( -0.9876526153536336894, -0.1566598588826349503, 0.000000000000000000 ) ) ;
#9547 = DIRECTION ( 'NONE',  ( -0.9876526153536336894, -0.1566598588826349503, 0.000000000000000000 ) ) ;
#9548 = ORIENTED_EDGE ( 'NONE', *, *, #7054, .T. ) ;
#9549 = CARTESIAN_POINT ( 'NONE',  ( -56.21322099054477661, -24.10372711620991026, 12.99038105676661736 ) ) ;
#9550 = CARTESIAN_POINT ( 'NONE',  ( -0.1213752363283457369, -20.26903809555066616, 17.32050807568881012 ) ) ;
#9551 = AXIS2_PLACEMENT_3D ( 'NONE', #10906, #13950, #3884 ) ;
#9552 = CYLINDRICAL_SURFACE ( 'NONE', #14142, 1.500000000000000666 ) ;
#9553 = EDGE_LOOP ( 'NONE', ( #15602, #16434 ) ) ;
#9554 = ORIENTED_EDGE ( 'NONE', *, *, #8121, .F. ) ;
#9555 = CYLINDRICAL_SURFACE ( 'NONE', #12301, 1.500000000000001554 ) ;
#9556 = ORIENTED_EDGE ( 'NONE', *, *, #10006, .T. ) ;
#9557 = DIRECTION ( 'NONE',  ( -0.9876526153536341335, -0.1566598588826327021, 0.000000000000000000 ) ) ;
#9558 = ORIENTED_EDGE ( 'NONE', *, *, #14153, .T. ) ;
#9559 = ORIENTED_EDGE ( 'NONE', *, *, #5834, .F. ) ;
#9560 = AXIS2_PLACEMENT_3D ( 'NONE', #12402, #18248, #8151 ) ;
#9561 = DIRECTION ( 'NONE',  ( -0.1566598588826321192, 0.9876526153536342445, 7.798540720466730171E-17 ) ) ;
#9562 = EDGE_CURVE ( 'NONE', #7482, #6188, #18327, .T. ) ;
#9563 = CARTESIAN_POINT ( 'NONE',  ( -55.42992169613161479, -29.04199019297804085, 21.65063509461101887 ) ) ;
#9564 = AXIS2_PLACEMENT_3D ( 'NONE', #556, #6350, #264 ) ;
#9565 = DIRECTION ( 'NONE',  ( -0.9876526153536336894, -0.1566598588826349503, 0.000000000000000000 ) ) ;
#9566 = DIRECTION ( 'NONE',  ( 0.000000000000000000, 0.000000000000000000, 1.000000000000000000 ) ) ;
#9567 = EDGE_CURVE ( 'NONE', #11513, #893, #5190, .T. ) ;
#9568 = DIRECTION ( 'NONE',  ( -0.000000000000000000, -0.000000000000000000, -1.000000000000000000 ) ) ;
#9569 = DIRECTION ( 'NONE',  ( -0.9876526153536336894, -0.1566598588826350336, 0.000000000000000000 ) ) ;
#9570 = DIRECTION ( 'NONE',  ( -0.9876526153536336894, -0.1566598588826349503, 0.000000000000000000 ) ) ;
#9571 = VERTEX_POINT ( 'NONE', #9543 ) ;
#9572 = DIRECTION ( 'NONE',  ( -0.1566598588826321747, 0.9876526153536343555, 0.000000000000000000 ) ) ;
#9573 = DIRECTION ( 'NONE',  ( 0.000000000000000000, 0.000000000000000000, 1.000000000000000000 ) ) ;
#9574 = AXIS2_PLACEMENT_3D ( 'NONE', #6661, #9400, #10791 ) ;
#9575 = EDGE_CURVE ( 'NONE', #2965, #9461, #16961, .T. ) ;
#9576 = CYLINDRICAL_SURFACE ( 'NONE', #17868, 1.500000000000000666 ) ;
#9577 = ORIENTED_EDGE ( 'NONE', *, *, #15762, .F. ) ;
#9578 = ORIENTED_EDGE ( 'NONE', *, *, #8908, .F. ) ;
#9579 = EDGE_LOOP ( 'NONE', ( #7056, #14903, #4185, #7932 ) ) ;
#9580 = FACE_OUTER_BOUND ( 'NONE', #10437, .T. ) ;
#9581 = FACE_BOUND ( 'NONE', #10196, .T. ) ;
#9582 = DIRECTION ( 'NONE',  ( 0.000000000000000000, 0.000000000000000000, 1.000000000000000000 ) ) ;
#9583 = VERTEX_POINT ( 'NONE', #10950 ) ;
#9584 = ADVANCED_FACE ( 'NONE', ( #13696 ), #426, .F. ) ;
#9585 = AXIS2_PLACEMENT_3D ( 'NONE', #11780, #13214, #4683 ) ;
#9586 = ORIENTED_EDGE ( 'NONE', *, *, #6582, .F. ) ;
#9587 = CIRCLE ( 'NONE', #13824, 145.0000000000000284 ) ;
#9588 = CARTESIAN_POINT ( 'NONE',  ( -70.00000000000000000, 44.99999999999999289, 20.00000000000002132 ) ) ;
#9589 = VERTEX_POINT ( 'NONE', #9453 ) ;
#9590 = CARTESIAN_POINT ( 'NONE',  ( -57.85941822433786541, -87.13282127653273790, -21.65063509461098690 ) ) ;
#9591 = CIRCLE ( 'NONE', #17184, 15.78184964806336055 ) ;
#9593 = EDGE_CURVE ( 'NONE', #44, #13932, #13782, .T. ) ;
#9592 = FACE_OUTER_BOUND ( 'NONE', #11002, .T. ) ;
#9594 = CARTESIAN_POINT ( 'NONE',  ( -28.26947477390680774, -24.73384407370567217, -8.660254037844380193 ) ) ;
#9595 = AXIS2_PLACEMENT_3D ( 'NONE', #18696, #11046, #11141 ) ;
#9596 = ORIENTED_EDGE ( 'NONE', *, *, #7179, .T. ) ;
#9597 = DIRECTION ( 'NONE',  ( 0.000000000000000000, 0.000000000000000000, 1.000000000000000000 ) ) ;
#9598 = EDGE_CURVE ( 'NONE', #334, #999, #10094, .T. ) ;
#9599 = ORIENTED_EDGE ( 'NONE', *, *, #16451, .T. ) ;
#9600 = DIRECTION ( 'NONE',  ( -0.9876526153536336894, -0.1566598588826349503, 0.000000000000000000 ) ) ;
#9601 = ORIENTED_EDGE ( 'NONE', *, *, #8817, .T. ) ;
#9602 = EDGE_LOOP ( 'NONE', ( #16467, #12569, #17140, #7660 ) ) ;
#9603 = CARTESIAN_POINT ( 'NONE',  ( -40.08167114797250719, -84.31294381664535820, 4.330127018922213189 ) ) ;
#9604 = AXIS2_PLACEMENT_3D ( 'NONE', #7166, #14162, #2598 ) ;
#9605 = STYLED_ITEM ( 'NONE', ( #17621 ), #16340 ) ;
#9606 = ORIENTED_EDGE ( 'NONE', *, *, #12042, .T. ) ;
#9607 = CARTESIAN_POINT ( 'NONE',  ( -2.000000000000000000, 2.449293598294706414E-16, -35.00000000000000000 ) ) ;
#9608 = AXIS2_PLACEMENT_3D ( 'NONE', #6408, #9226, #2023 ) ;
#9609 = CARTESIAN_POINT ( 'NONE',  ( -23.33121169713865584, -23.95054477929251036, 1.869203119972154228E-14 ) ) ;
#9610 = ORIENTED_EDGE ( 'NONE', *, *, #11854, .T. ) ;
#9611 = FACE_BOUND ( 'NONE', #10775, .T. ) ;
#9612 = AXIS2_PLACEMENT_3D ( 'NONE', #15732, #2755, #14113 ) ;
#9613 = CYLINDRICAL_SURFACE ( 'NONE', #18558, 150.0000000000000000 ) ;
#9614 = DIRECTION ( 'NONE',  ( -0.1566598588826321192, 0.9876526153536342445, 7.798540720466731404E-17 ) ) ;
#9615 = FACE_BOUND ( 'NONE', #8724, .T. ) ;
#9616 = DIRECTION ( 'NONE',  ( 1.000000000000000000, 0.000000000000000000, 0.000000000000000000 ) ) ;
#9617 = ADVANCED_FACE ( 'NONE', ( #14082 ), #14182, .F. ) ;
#9618 = EDGE_CURVE ( 'NONE', #18673, #14612, #12512, .T. ) ;
#9619 = CARTESIAN_POINT ( 'NONE',  ( -56.37793930130741415, -86.89783148820880854, 12.99038105676661203 ) ) ;
#9620 = DIRECTION ( 'NONE',  ( -3.039628882124824168E-17, -0.000000000000000000, 1.000000000000000000 ) ) ;
#9621 = VERTEX_POINT ( 'NONE', #7009 ) ;
#9622 = CIRCLE ( 'NONE', #12007, 1.500000000000001332 ) ;
#9624 = ADVANCED_FACE ( 'NONE', ( #12751 ), #6905, .F. ) ;
#9623 = CARTESIAN_POINT ( 'NONE',  ( -72.71384246482016067, -31.78353772342409300, 1.869203119972154228E-14 ) ) ;
#9625 = DIRECTION ( 'NONE',  ( 3.039628882124824168E-17, 0.000000000000000000, -1.000000000000000000 ) ) ;
#9626 = ORIENTED_EDGE ( 'NONE', *, *, #7093, .T. ) ;
#9627 = ORIENTED_EDGE ( 'NONE', *, *, #7520, .T. ) ;
#9628 = CYLINDRICAL_SURFACE ( 'NONE', #5139, 2.000000000000000000 ) ;
#9629 = CARTESIAN_POINT ( 'NONE',  ( 2.881217619910392269, -77.49823995525089515, 21.65063509461100821 ) ) ;
#9630 = ORIENTED_EDGE ( 'NONE', *, *, #10314, .F. ) ;
#9631 = ADVANCED_FACE ( 'NONE', ( #11236 ), #18604, .F. ) ;
#9632 = VERTEX_POINT ( 'NONE', #17055 ) ;
#9633 = AXIS2_PLACEMENT_3D ( 'NONE', #14590, #1616, #7396 ) ;
#9634 = CARTESIAN_POINT ( 'NONE',  ( -74.48479437458692587, -27.00193450553858909, -12.99038105676658006 ) ) ;
#9635 = VERTEX_POINT ( 'NONE', #9824 ) ;
#9636 = ORIENTED_EDGE ( 'NONE', *, *, #12142, .T. ) ;
#9637 = LINE ( 'NONE', #16955, #10616 ) ;
#9638 = AXIS2_PLACEMENT_3D ( 'NONE', #17034, #16747, #3718 ) ;
#9639 = CARTESIAN_POINT ( 'NONE',  ( -72.71384246482016067, -31.78353772342409300, -17.32050807568878170 ) ) ;
#9640 = CARTESIAN_POINT ( 'NONE',  ( -27.73601345605213098, -82.35469558061245721, 7.492215382409427462E-15 ) ) ;
#9641 = FACE_OUTER_BOUND ( 'NONE', #13742, .T. ) ;
#9642 = DIRECTION ( 'NONE',  ( -0.1566598588826321192, 0.9876526153536342445, 7.798540720466730171E-17 ) ) ;
#9643 = CARTESIAN_POINT ( 'NONE',  ( -56.41757431148524660, -29.19865005186066043, 8.660254037844417496 ) ) ;
#9644 = FACE_OUTER_BOUND ( 'NONE', #18562, .T. ) ;
#9645 = ADVANCED_FACE ( 'NONE', ( #2714 ), #5475, .F. ) ;
#9646 = CARTESIAN_POINT ( 'NONE',  ( 73.09088021254186174, 1.387778780781445676E-14, -19.99999999999999645 ) ) ;
#9647 = ORIENTED_EDGE ( 'NONE', *, *, #5975, .F. ) ;
#9649 = DIRECTION ( 'NONE',  ( -0.9876526153536341335, -0.1566598588826327576, 0.000000000000000000 ) ) ;
#9648 = AXIS2_PLACEMENT_3D ( 'NONE', #3728, #9529, #15302 ) ;
#9650 = CIRCLE ( 'NONE', #16001, 1.500000000000000888 ) ;
#9651 = DIRECTION ( 'NONE',  ( -0.1566598588826321192, 0.9876526153536342445, 7.798540720466730171E-17 ) ) ;
#9652 = DIRECTION ( 'NONE',  ( -0.1566598588826321192, 0.9876526153536342445, 7.798540720466731404E-17 ) ) ;
#9653 = CIRCLE ( 'NONE', #17548, 1.500000000000001332 ) ;
#9654 = CARTESIAN_POINT ( 'NONE',  ( -77.83224521979003896, 0.3113578409232161670, 4.597830265575576725 ) ) ;
#9656 = VERTEX_POINT ( 'NONE', #15690 ) ;
#9655 = CARTESIAN_POINT ( 'NONE',  ( -30.20514499443620338, -82.74634522781904877, 12.99038105676661203 ) ) ;
#9657 = EDGE_CURVE ( 'NONE', #3651, #5894, #16630, .T. ) ;
#9658 = EDGE_CURVE ( 'NONE', #3705, #5412, #3614, .T. ) ;
#9659 = FACE_OUTER_BOUND ( 'NONE', #9756, .T. ) ;
#9660 = CARTESIAN_POINT ( 'NONE',  ( -60.36818477289978091, -29.82528948739120267, -4.330127018922181215 ) ) ;
#9661 = ORIENTED_EDGE ( 'NONE', *, *, #2973, .F. ) ;
#9662 = ORIENTED_EDGE ( 'NONE', *, *, #9782, .F. ) ;
#9663 = VECTOR ( 'NONE', #5526, 1000.000000000000000 ) ;
#9664 = CIRCLE ( 'NONE', #15099, 1.499999999999999556 ) ;
#9665 = DIRECTION ( 'NONE',  ( 3.039628882124824168E-17, 0.000000000000000000, -1.000000000000000000 ) ) ;
#9666 = EDGE_LOOP ( 'NONE', ( #17208, #9057 ) ) ;
#9667 = CIRCLE ( 'NONE', #7271, 1.500000000000001332 ) ;
#9668 = DIRECTION ( 'NONE',  ( -0.1566598588826321192, 0.9876526153536342445, 7.798540720466730171E-17 ) ) ;
#9669 = AXIS2_PLACEMENT_3D ( 'NONE', #3281, #9082, #16396 ) ;
#9670 = DIRECTION ( 'NONE',  ( 0.000000000000000000, 0.000000000000000000, -1.000000000000000000 ) ) ;
#9671 = FACE_OUTER_BOUND ( 'NONE', #3811, .T. ) ;
#9672 = DIRECTION ( 'NONE',  ( -0.1566598588826321192, 0.9876526153536342445, 7.798540720466730171E-17 ) ) ;
#9673 = CARTESIAN_POINT ( 'NONE',  ( -51.27495791377664602, -23.32042782179673779, -21.65063509461097979 ) ) ;
#9674 = CARTESIAN_POINT ( 'NONE',  ( 2.058283315319403783, -14.86079544213463066, 17.32050807568881012 ) ) ;
#9675 = CARTESIAN_POINT ( 'NONE',  ( -127.6813802953510333, 9.532733159319212390, -2.918139657044711122 ) ) ;
#9676 = CARTESIAN_POINT ( 'NONE',  ( -79.24244631363546887, 32.81909429640987952, 25.00000000000001776 ) ) ;
#9677 = CIRCLE ( 'NONE', #17567, 1.500000000000000000 ) ;
#9678 = CARTESIAN_POINT ( 'NONE',  ( -5.000000000000000000, 6.123233995736766282E-16, 35.00000000000000000 ) ) ;
#9679 = DIRECTION ( 'NONE',  ( 0.000000000000000000, 0.000000000000000000, 1.000000000000000000 ) ) ;
#9680 = VECTOR ( 'NONE', #8161, 1000.000000000000000 ) ;
#9681 = EDGE_CURVE ( 'NONE', #14889, #211, #48, .T. ) ;
#9682 = AXIS2_PLACEMENT_3D ( 'NONE', #13508, #17930, #6348 ) ;
#9683 = ORIENTED_EDGE ( 'NONE', *, *, #10062, .F. ) ;
#9684 = DIRECTION ( 'NONE',  ( -0.1566598588826321747, 0.9876526153536343555, 0.000000000000000000 ) ) ;
#9685 = EDGE_CURVE ( 'NONE', #9589, #11379, #9514, .T. ) ;
#9686 = EDGE_CURVE ( 'NONE', #3473, #5485, #3385, .T. ) ;
#9687 = AXIS2_PLACEMENT_3D ( 'NONE', #16078, #10179, #13032 ) ;
#9688 = CIRCLE ( 'NONE', #8433, 1.500000000000000444 ) ;
#9689 = AXIS2_PLACEMENT_3D ( 'NONE', #1550, #17576, #10333 ) ;
#9690 = VERTEX_POINT ( 'NONE', #5251 ) ;
#9691 = ORIENTED_EDGE ( 'NONE', *, *, #10082, .F. ) ;
#9692 = ORIENTED_EDGE ( 'NONE', *, *, #8209, .F. ) ;
#9693 = DIRECTION ( 'NONE',  ( -0.9876526153536336894, -0.1566598588826349503, 0.000000000000000000 ) ) ;
#9694 = ADVANCED_FACE ( 'NONE', ( #2298 ), #18282, .F. ) ;
#9695 = ORIENTED_EDGE ( 'NONE', *, *, #3449, .F. ) ;
#9696 = FACE_BOUND ( 'NONE', #11268, .T. ) ;
#9697 = AXIS2_PLACEMENT_3D ( 'NONE', #16105, #5875, #7392 ) ;
#9698 = DIRECTION ( 'NONE',  ( -0.1566598588826321192, 0.9876526153536342445, 7.798540720466730171E-17 ) ) ;
#9699 = AXIS2_PLACEMENT_3D ( 'NONE', #322, #11754, #3421 ) ;
#9700 = ORIENTED_EDGE ( 'NONE', *, *, #339, .T. ) ;
#9701 = AXIS2_PLACEMENT_3D ( 'NONE', #7730, #6324, #2131 ) ;
#9702 = AXIS2_PLACEMENT_3D ( 'NONE', #13637, #17845, #4823 ) ;
#9703 = CARTESIAN_POINT ( 'NONE',  ( -56.91140061916208737, -29.27697998130198442, -21.65063509461098334 ) ) ;
#9704 = EDGE_LOOP ( 'NONE', ( #14746, #13830 ) ) ;
#9705 = CARTESIAN_POINT ( 'NONE',  ( -131.1055737289773617, -2.850701963179330445, 15.78184964806336055 ) ) ;
#9706 = DIRECTION ( 'NONE',  ( 1.000000000000000000, 8.260059303211164661E-14, 0.000000000000000000 ) ) ;
#9707 = DIRECTION ( 'NONE',  ( 0.000000000000000000, 0.000000000000000000, 1.000000000000000000 ) ) ;
#9708 = DIRECTION ( 'NONE',  ( -0.1566598588826321192, 0.9876526153536342445, 7.798540720466731404E-17 ) ) ;
#9709 = AXIS2_PLACEMENT_3D ( 'NONE', #8526, #18704, #82 ) ;
#9710 = CARTESIAN_POINT ( 'NONE',  ( -50.49165861936347710, -28.25869089856488614, 4.330127018922217630 ) ) ;
#9711 = CARTESIAN_POINT ( 'NONE',  ( -52.42732883989288695, -86.27119205267824498, -17.32050807568878525 ) ) ;
#9712 = CIRCLE ( 'NONE', #6684, 1.500000000000000888 ) ;
#9713 = LINE ( 'NONE', #15480, #17210 ) ;
#9714 = ORIENTED_EDGE ( 'NONE', *, *, #5446, .F. ) ;
#9715 = EDGE_LOOP ( 'NONE', ( #6228, #6917, #3826, #13079 ) ) ;
#9716 = AXIS2_PLACEMENT_3D ( 'NONE', #49, #14445, #1473 ) ;
#9717 = CYLINDRICAL_SURFACE ( 'NONE', #15780, 1.500000000000001554 ) ;
#9718 = ADVANCED_FACE ( 'NONE', ( #12440 ), #9717, .F. ) ;
#9719 = AXIS2_PLACEMENT_3D ( 'NONE', #5754, #8309, #12836 ) ;
#9720 = ORIENTED_EDGE ( 'NONE', *, *, #712, .F. ) ;
#9721 = DIRECTION ( 'NONE',  ( -0.1566598588826321192, 0.9876526153536342445, 7.798540720466730171E-17 ) ) ;
#9722 = CARTESIAN_POINT ( 'NONE',  ( -170.4538399828638831, 32.22998840342273041, 4.764204982952881196 ) ) ;
#9723 = CARTESIAN_POINT ( 'NONE',  ( -33.99103714508810725, -20.57888029135068919, -8.660254037844380193 ) ) ;
#9724 = ADVANCED_FACE ( 'NONE', ( #12233 ), #10915, .F. ) ;
#9725 = CIRCLE ( 'NONE', #7016, 1.500000000000001332 ) ;
#9726 = EDGE_CURVE ( 'NONE', #14841, #777, #11518, .T. ) ;
#9727 = CIRCLE ( 'NONE', #1554, 1.499999999999999556 ) ;
#9728 = DIRECTION ( 'NONE',  ( -0.1566598588826321192, 0.9876526153536342445, 7.798540720466730171E-17 ) ) ;
#9729 = CARTESIAN_POINT ( 'NONE',  ( -63.78533391645962780, -88.07278042982852639, -17.32050807568878525 ) ) ;
#9730 = LINE ( 'NONE', #13867, #5365 ) ;
#9731 = ORIENTED_EDGE ( 'NONE', *, *, #7989, .T. ) ;
#9732 = CARTESIAN_POINT ( 'NONE',  ( 55.85952145814821534, 6.938893903907228378E-15, 35.00000000000000000 ) ) ;
#9733 = VECTOR ( 'NONE', #5653, 1000.000000000000000 ) ;
#9734 = CARTESIAN_POINT ( 'NONE',  ( -5.842937607509656850, -16.11407431319567962, 1.561251128379126385E-14 ) ) ;
#9735 = ORIENTED_EDGE ( 'NONE', *, *, #11331, .F. ) ;
#9736 = ORIENTED_EDGE ( 'NONE', *, *, #8270, .T. ) ;
#9737 = CARTESIAN_POINT ( 'NONE',  ( -31.52190560670403841, -20.18723064414410828, -21.65063509461097979 ) ) ;
#9738 = ORIENTED_EDGE ( 'NONE', *, *, #952, .T. ) ;
#9739 = CIRCLE ( 'NONE', #1859, 1.500000000000000888 ) ;
#9740 = VERTEX_POINT ( 'NONE', #13852 ) ;
#9741 = DIRECTION ( 'NONE',  ( -0.9876526153536336894, -0.1566598588826349503, 0.000000000000000000 ) ) ;
#9742 = EDGE_CURVE ( 'NONE', #13568, #14760, #10058, .T. ) ;
#9743 = VECTOR ( 'NONE', #8191, 1000.000000000000000 ) ;
#9744 = ADVANCED_FACE ( 'NONE', ( #3796 ), #2393, .F. ) ;
#9745 = DIRECTION ( 'NONE',  ( -0.1566598588826321192, 0.9876526153536342445, 7.798540720466731404E-17 ) ) ;
#9746 = EDGE_CURVE ( 'NONE', #8251, #1703, #18245, .T. ) ;
#9747 = ORIENTED_EDGE ( 'NONE', *, *, #16548, .F. ) ;
#9748 = FACE_OUTER_BOUND ( 'NONE', #317, .T. ) ;
#9749 = LINE ( 'NONE', #12477, #15236 ) ;
#9750 = CARTESIAN_POINT ( 'NONE',  ( -62.79768130110601021, -87.91612057094590682, -4.330127018922185655 ) ) ;
#9751 = CIRCLE ( 'NONE', #12126, 139.0000000000000000 ) ;
#9752 = CARTESIAN_POINT ( 'NONE',  ( -78.43540483600145308, -27.62857394106911713, 1.908195823574487804E-14 ) ) ;
#9753 = ORIENTED_EDGE ( 'NONE', *, *, #3899, .T. ) ;
#9754 = CARTESIAN_POINT ( 'NONE',  ( -14.44233815895597672, -22.54060604934882051, -4.330127018922181215 ) ) ;
#9755 = LINE ( 'NONE', #4123, #15634 ) ;
#9756 = EDGE_LOOP ( 'NONE', ( #18372, #8203, #16661, #17766 ) ) ;
#9757 = DIRECTION ( 'NONE',  ( 1.000000000000000000, 0.000000000000000000, -2.478176394252581634E-16 ) ) ;
#9758 = DIRECTION ( 'NONE',  ( -0.1566598588826321747, 0.9876526153536343555, 0.000000000000000000 ) ) ;
#9759 = VERTEX_POINT ( 'NONE', #5343 ) ;
#9760 = AXIS2_PLACEMENT_3D ( 'NONE', #17668, #3200, #14777 ) ;
#9761 = CARTESIAN_POINT ( 'NONE',  ( 73.09088021254186174, 1.387778780781445676E-14, 110.7545852194966045 ) ) ;
#9762 = VERTEX_POINT ( 'NONE', #11197 ) ;
#9763 = AXIS2_PLACEMENT_3D ( 'NONE', #6277, #6553, #12111 ) ;
#9764 = EDGE_CURVE ( 'NONE', #10224, #3227, #8524, .T. ) ;
#9765 = DIRECTION ( 'NONE',  ( -0.9876526153536341335, -0.1566598588826327021, 0.000000000000000000 ) ) ;
#9766 = CIRCLE ( 'NONE', #7354, 1.500000000000000888 ) ;
#9767 = CARTESIAN_POINT ( 'NONE',  ( -18.35331361019266794, -80.86642692122747178, -4.330127018922185655 ) ) ;
#9768 = CARTESIAN_POINT ( 'NONE',  ( -43.04462899403339549, -84.78292339329328797, 21.65063509461101532 ) ) ;
#9769 = DIRECTION ( 'NONE',  ( -0.1566598588826321192, 0.9876526153536342445, 7.798540720466731404E-17 ) ) ;
#9770 = FACE_OUTER_BOUND ( 'NONE', #17631, .T. ) ;
#9771 = DIRECTION ( 'NONE',  ( 0.000000000000000000, 0.000000000000000000, 1.000000000000000000 ) ) ;
#9772 = DIRECTION ( 'NONE',  ( -0.1566598588826321192, 0.9876526153536342445, 7.798540720466730171E-17 ) ) ;
#9773 = DIRECTION ( 'NONE',  ( 1.000000000000000000, 0.000000000000000000, 0.000000000000000000 ) ) ;
#9774 = CARTESIAN_POINT ( 'NONE',  ( -24.27922930231443743, -81.80638607452326028, -8.660254037844385522 ) ) ;
#9775 = AXIS2_PLACEMENT_3D ( 'NONE', #18156, #885, #18355 ) ;
#9776 = ORIENTED_EDGE ( 'NONE', *, *, #9033, .T. ) ;
#9777 = ORIENTED_EDGE ( 'NONE', *, *, #18780, .F. ) ;
#9778 = DIRECTION ( 'NONE',  ( -0.9876526153536344665, -0.1566598588826304539, 0.000000000000000000 ) ) ;
#9779 = FACE_BOUND ( 'NONE', #9270, .T. ) ;
#9780 = DIRECTION ( 'NONE',  ( 0.9201637183752249260, 0.3915338189555018777, 0.000000000000000000 ) ) ;
#9781 = ORIENTED_EDGE ( 'NONE', *, *, #12823, .F. ) ;
#9782 = EDGE_CURVE ( 'NONE', #16555, #3259, #2503, .T. ) ;
#9783 = EDGE_CURVE ( 'NONE', #13246, #862, #15380, .T. ) ;
#9784 = AXIS2_PLACEMENT_3D ( 'NONE', #12803, #1357, #20 ) ;
#9785 = LINE ( 'NONE', #2379, #16309 ) ;
#9786 = LINE ( 'NONE', #2571, #11833 ) ;
#9787 = ORIENTED_EDGE ( 'NONE', *, *, #2090, .F. ) ;
#9788 = ADVANCED_FACE ( 'NONE', ( #13959 ), #17020, .F. ) ;
#9789 = CARTESIAN_POINT ( 'NONE',  ( -14.40270314877813895, -80.23978748569695085, -8.660254037844385522 ) ) ;
#9790 = CARTESIAN_POINT ( 'NONE',  ( -49.50400600400985240, -28.10203103968224880, 17.32050807568881723 ) ) ;
#9791 = CARTESIAN_POINT ( 'NONE',  ( 3.231158466157551423, 19.73726462726227737, 35.00000000000000000 ) ) ;
#9792 = DIRECTION ( 'NONE',  ( -0.1566598588826321747, 0.9876526153536343555, 0.000000000000000000 ) ) ;
#9793 = ORIENTED_EDGE ( 'NONE', *, *, #4063, .T. ) ;
#9794 = VERTEX_POINT ( 'NONE', #12614 ) ;
#9795 = ORIENTED_EDGE ( 'NONE', *, *, #12756, .T. ) ;
#9796 = EDGE_LOOP ( 'NONE', ( #11375, #5134, #1883, #10825, #11294 ) ) ;
#9797 = DIRECTION ( 'NONE',  ( -0.1566598588826321192, 0.9876526153536342445, 7.798540720466731404E-17 ) ) ;
#9798 = CIRCLE ( 'NONE', #14642, 145.0000000000000284 ) ;
#9799 = ORIENTED_EDGE ( 'NONE', *, *, #17051, .F. ) ;
#9800 = EDGE_LOOP ( 'NONE', ( #10618, #7458 ) ) ;
#9801 = CARTESIAN_POINT ( 'NONE',  ( -128.8620198725178909, -14.87463575837847962, 4.223374618371430245 ) ) ;
#9802 = CARTESIAN_POINT ( 'NONE',  ( -10.28737437660098308, -16.81904367816752810, -21.65063509461098334 ) ) ;
#9803 = CARTESIAN_POINT ( 'NONE',  ( -77.44775222064782838, -27.47191408218648334, -4.330127018922180326 ) ) ;
#9804 = UNCERTAINTY_MEASURE_WITH_UNIT (LENGTH_MEASURE( 1.000000000000000082E-05 ), #13864, 'distance_accuracy_value', 'NONE');
#9805 = CARTESIAN_POINT ( 'NONE',  ( -71.57226172492416083, 45.66900446655741774, 3.728993592375226207 ) ) ;
#9806 = EDGE_CURVE ( 'NONE', #13271, #3138, #17321, .T. ) ;
#9807 = CARTESIAN_POINT ( 'NONE',  ( -15.39035576413176187, -80.39644734457958464, 12.99038105676661203 ) ) ;
#9808 = DIRECTION ( 'NONE',  ( -0.1566598588826321192, 0.9876526153536342445, 7.798540720466731404E-17 ) ) ;
#9809 = DIRECTION ( 'NONE',  ( 0.000000000000000000, 0.000000000000000000, 1.000000000000000000 ) ) ;
#9810 = CARTESIAN_POINT ( 'NONE',  ( -306.1404785418517918, -2.850701963179326892, -12.83663829214475882 ) ) ;
#9811 = ORIENTED_EDGE ( 'NONE', *, *, #10711, .F. ) ;
#9812 = CARTESIAN_POINT ( 'NONE',  ( -45.55339554259532520, -27.47539160415171722, 4.330127018922217630 ) ) ;
#9813 = CARTESIAN_POINT ( 'NONE',  ( -51.47931123471710890, -28.41535075744750571, 8.660254037844417496 ) ) ;
#9814 = EDGE_CURVE ( 'NONE', #10257, #2545, #16092, .T. ) ;
#9815 = ORIENTED_EDGE ( 'NONE', *, *, #11791, .F. ) ;
#9816 = LINE ( 'NONE', #6120, #18519 ) ;
#9817 = EDGE_CURVE ( 'NONE', #1132, #10224, #16435, .T. ) ;
#9818 = VERTEX_POINT ( 'NONE', #10151 ) ;
#9819 = DIRECTION ( 'NONE',  ( 0.000000000000000000, 0.000000000000000000, 1.000000000000000000 ) ) ;
#9820 = VERTEX_POINT ( 'NONE', #15941 ) ;
#9821 = FACE_OUTER_BOUND ( 'NONE', #18119, .T. ) ;
#9822 = EDGE_LOOP ( 'NONE', ( #964, #7200, #8758, #15631 ) ) ;
#9823 = DIRECTION ( 'NONE',  ( -1.000000000000000000, 0.000000000000000000, 0.000000000000000000 ) ) ;
#9824 = CARTESIAN_POINT ( 'NONE',  ( 5.275328570166844017E-15, 2.199999999999993072, 20.00000000000000000 ) ) ;
#9825 = CIRCLE ( 'NONE', #2251, 1.500000000000000444 ) ;
#9826 = CARTESIAN_POINT ( 'NONE',  ( 1.399738696879940791, -77.73322974357483872, -4.330127018922189208 ) ) ;
#9827 = FILL_AREA_STYLE ('',( #5768 ) ) ;
#9828 = ORIENTED_EDGE ( 'NONE', *, *, #9542, .F. ) ;
#9829 = ADVANCED_FACE ( 'NONE', ( #17478 ), #15652, .F. ) ;
#9830 = EDGE_CURVE ( 'NONE', #11150, #10784, #341, .T. ) ;
#9831 = CARTESIAN_POINT ( 'NONE',  ( -76.66445292623467367, -32.41017715895461038, 12.99038105676661736 ) ) ;
#9832 = FACE_OUTER_BOUND ( 'NONE', #13372, .T. ) ;
#9833 = DIRECTION ( 'NONE',  ( 0.000000000000000000, 0.000000000000000000, 1.000000000000000000 ) ) ;
#9834 = CARTESIAN_POINT ( 'NONE',  ( 55.85952145814821534, 6.938893903907228378E-15, 35.00000000000000000 ) ) ;
#9835 = ORIENTED_EDGE ( 'NONE', *, *, #9030, .F. ) ;
#9836 = DIRECTION ( 'NONE',  ( 0.000000000000000000, 0.000000000000000000, 1.000000000000000000 ) ) ;
#9837 = ORIENTED_EDGE ( 'NONE', *, *, #683, .T. ) ;
#9838 = DIRECTION ( 'NONE',  ( -0.1566598588826321192, 0.9876526153536342445, 7.798540720466730171E-17 ) ) ;
#9839 = ORIENTED_EDGE ( 'NONE', *, *, #15991, .F. ) ;
#9840 = EDGE_CURVE ( 'NONE', #859, #3849, #5504, .T. ) ;
#9841 = VECTOR ( 'NONE', #4879, 1000.000000000000000 ) ;
#9842 = ORIENTED_EDGE ( 'NONE', *, *, #2462, .T. ) ;
#9843 = ORIENTED_EDGE ( 'NONE', *, *, #8817, .F. ) ;
#9844 = DIRECTION ( 'NONE',  ( 0.000000000000000000, 0.000000000000000000, 1.000000000000000000 ) ) ;
#9845 = DIRECTION ( 'NONE',  ( 0.1856185419698759831, -0.9826218788918641422, 0.000000000000000000 ) ) ;
#9846 = DIRECTION ( 'NONE',  ( -1.000000000000000000, 0.000000000000000000, -0.000000000000000000 ) ) ;
#9847 = LINE ( 'NONE', #9768, #4577 ) ;
#9848 = DIRECTION ( 'NONE',  ( -1.000000000000000000, 0.000000000000000000, 0.000000000000000000 ) ) ;
#9849 = DIRECTION ( 'NONE',  ( -0.1566598588826321192, 0.9876526153536342445, 7.798540720466730171E-17 ) ) ;
#9850 = CIRCLE ( 'NONE', #8926, 1.500000000000000444 ) ;
#9851 = CARTESIAN_POINT ( 'NONE',  ( 73.09088021254186174, 1.387778780781445676E-14, 25.00000000000000000 ) ) ;
#9852 = EDGE_CURVE ( 'NONE', #11472, #13816, #8743, .T. ) ;
#9853 = FACE_BOUND ( 'NONE', #9021, .T. ) ;
#9854 = EDGE_CURVE ( 'NONE', #16090, #15832, #2769, .T. ) ;
#9855 = CYLINDRICAL_SURFACE ( 'NONE', #4432, 1.500000000000001554 ) ;
#9856 = EDGE_CURVE ( 'NONE', #17593, #11470, #14859, .T. ) ;
#9857 = VERTEX_POINT ( 'NONE', #16043 ) ;
#9858 = CARTESIAN_POINT ( 'NONE',  ( -31.68662391746665463, -82.98133501614300656, 4.330127018922213189 ) ) ;
#9859 = PRODUCT_DEFINITION_SHAPE ( 'NONE', 'NONE',  #18800 ) ;
#9860 = ORIENTED_EDGE ( 'NONE', *, *, #2510, .F. ) ;
#9861 = ORIENTED_EDGE ( 'NONE', *, *, #16081, .F. ) ;
#9862 = CARTESIAN_POINT ( 'NONE',  ( -48.97054468615519340, -85.72288254658904805, 1.424741226644455312E-14 ) ) ;
#9863 = VECTOR ( 'NONE', #6772, 1000.000000000000114 ) ;
#9864 = FACE_BOUND ( 'NONE', #17828, .T. ) ;
#9865 = FILL_AREA_STYLE_COLOUR ( '', #8866 ) ;
#9866 = DIRECTION ( 'NONE',  ( -0.000000000000000000, -0.000000000000000000, -1.000000000000000000 ) ) ;
#9867 = ORIENTED_EDGE ( 'NONE', *, *, #3615, .F. ) ;
#9868 = EDGE_LOOP ( 'NONE', ( #13108, #11358 ) ) ;
#9869 = CYLINDRICAL_SURFACE ( 'NONE', #5296, 1.500000000000001554 ) ;
#9870 = AXIS2_PLACEMENT_3D ( 'NONE', #14494, #1520, #7311 ) ;
#9871 = CARTESIAN_POINT ( 'NONE',  ( -32.22008523532134205, -25.36048350923618955, -4.330127018922181215 ) ) ;
#9872 = DIRECTION ( 'NONE',  ( -0.1566598588826321192, 0.9876526153536342445, 7.798540720466730171E-17 ) ) ;
#9873 = CYLINDRICAL_SURFACE ( 'NONE', #14504, 1.500000000000001554 ) ;
#9874 = EDGE_LOOP ( 'NONE', ( #5702, #800 ) ) ;
#9875 = EDGE_CURVE ( 'NONE', #3975, #17212, #5537, .T. ) ;
#9876 = ORIENTED_EDGE ( 'NONE', *, *, #18283, .T. ) ;
#9877 = VERTEX_POINT ( 'NONE', #18744 ) ;
#9878 = CARTESIAN_POINT ( 'NONE',  ( -306.1404785418517918, -2.850701963179326892, -12.83663829214475882 ) ) ;
#9879 = EDGE_CURVE ( 'NONE', #2139, #5465, #1561, .T. ) ;
#9880 = ORIENTED_EDGE ( 'NONE', *, *, #4965, .F. ) ;
#9881 = CARTESIAN_POINT ( 'NONE',  ( -59.79999999999999716, 0.000000000000000000, -25.00000000000000000 ) ) ;
#9882 = CARTESIAN_POINT ( 'NONE',  ( 55.85952145814821534, 6.938893903907228378E-15, 29.99999999999998579 ) ) ;
#9883 = TOROIDAL_SURFACE ( 'NONE', #18411, 3.000000000000000000, 2.000000000000000000 ) ;
#9884 = CARTESIAN_POINT ( 'NONE',  ( -56.37793930130741415, -86.89783148820879433, -21.65063509461098690 ) ) ;
#9885 = DIRECTION ( 'NONE',  ( -0.9876526153536341335, -0.1566598588826327021, 0.000000000000000000 ) ) ;
#9886 = CONTEXT_DEPENDENT_SHAPE_REPRESENTATION ( #15596, #4088 ) ;
#9887 = CIRCLE ( 'NONE', #3836, 1.500000000000000888 ) ;
#9888 = CIRCLE ( 'NONE', #1723, 1.500000000000000888 ) ;
#9889 = DIRECTION ( 'NONE',  ( -0.1566598588826321192, 0.9876526153536342445, 7.798540720466731404E-17 ) ) ;
#9890 = CARTESIAN_POINT ( 'NONE',  ( -10.98555400521827963, -21.99229654325962002, -12.99038105676658006 ) ) ;
#9891 = ORIENTED_EDGE ( 'NONE', *, *, #18047, .T. ) ;
#9892 = DIRECTION ( 'NONE',  ( -0.1566598588826321192, 0.9876526153536342445, 7.798540720466731404E-17 ) ) ;
#9893 = CYLINDRICAL_SURFACE ( 'NONE', #3762, 5.000000000000004441 ) ;
#9894 = ORIENTED_EDGE ( 'NONE', *, *, #2489, .T. ) ;
#9895 = VERTEX_POINT ( 'NONE', #5905 ) ;
#9896 = CARTESIAN_POINT ( 'NONE',  ( -90.00000000000000000, 34.99999999999999289, 35.00000000000000000 ) ) ;
#9897 = DIRECTION ( 'NONE',  ( 0.000000000000000000, 0.000000000000000000, 1.000000000000000000 ) ) ;
#9898 = EDGE_CURVE ( 'NONE', #11379, #18705, #8823, .T. ) ;
#9899 = CIRCLE ( 'NONE', #11974, 1.500000000000000444 ) ;
#9900 = ORIENTED_EDGE ( 'NONE', *, *, #17812, .T. ) ;
#9901 = DIRECTION ( 'NONE',  ( -0.1566598588826321192, 0.9876526153536342445, 7.798540720466730171E-17 ) ) ;
#9902 = AXIS2_PLACEMENT_3D ( 'NONE', #13297, #11864, #17703 ) ;
#9903 = EDGE_CURVE ( 'NONE', #44, #8498, #13345, .T. ) ;
#9904 = DIRECTION ( 'NONE',  ( -0.9876526153536336894, -0.1566598588826349503, 0.000000000000000000 ) ) ;
#9905 = DIRECTION ( 'NONE',  ( -0.000000000000000000, -0.000000000000000000, -1.000000000000000000 ) ) ;
#9906 = DIRECTION ( 'NONE',  ( 0.000000000000000000, 0.000000000000000000, 1.000000000000000000 ) ) ;
#9907 = DIRECTION ( 'NONE',  ( -1.000000000000000000, 0.000000000000000000, 0.000000000000000000 ) ) ;
#9908 = CYLINDRICAL_SURFACE ( 'NONE', #13844, 1.500000000000001554 ) ;
#9909 = VECTOR ( 'NONE', #6823, 1000.000000000000000 ) ;
#9910 = DIRECTION ( 'NONE',  ( -0.1566598588826321192, 0.9876526153536342445, 7.798540720466731404E-17 ) ) ;
#9911 = CARTESIAN_POINT ( 'NONE',  ( -29.05277406831996245, -19.79558099693753093, -8.660254037844380193 ) ) ;
#9912 = ORIENTED_EDGE ( 'NONE', *, *, #12791, .T. ) ;
#9913 = DIRECTION ( 'NONE',  ( -1.000000000000000000, 0.000000000000000000, 0.000000000000000000 ) ) ;
#9914 = CARTESIAN_POINT ( 'NONE',  ( -17.69476899175320739, -17.99399261978727438, 1.926565525561698076E-14 ) ) ;
#9915 = ORIENTED_EDGE ( 'NONE', *, *, #14727, .F. ) ;
#9916 = CARTESIAN_POINT ( 'NONE',  ( -1.892327146095121204, -15.48743487766515337, 12.99038105676661026 ) ) ;
#9917 = CARTESIAN_POINT ( 'NONE',  ( -77.24751462517671996, -0.7168438680194959556, 5.646068113733807792 ) ) ;
#9919 = EDGE_LOOP ( 'NONE', ( #1717, #1650 ) ) ;
#9918 = DIRECTION ( 'NONE',  ( 0.000000000000000000, 0.000000000000000000, 1.000000000000000000 ) ) ;
#9920 = ORIENTED_EDGE ( 'NONE', *, *, #14373, .T. ) ;
#9921 = CARTESIAN_POINT ( 'NONE',  ( -8.516422466834198346, -21.60064689605303911, -8.660254037844380193 ) ) ;
#9922 = ORIENTED_EDGE ( 'NONE', *, *, #9783, .T. ) ;
#9923 = EDGE_LOOP ( 'NONE', ( #12433, #11354, #401, #2211 ) ) ;
#9924 = CIRCLE ( 'NONE', #2952, 1.500000000000000000 ) ;
#9925 = EDGE_CURVE ( 'NONE', #4082, #3282, #5811, .T. ) ;
#9926 = DIRECTION ( 'NONE',  ( -0.1566598588826321747, 0.9876526153536343555, 0.000000000000000000 ) ) ;
#9927 = CARTESIAN_POINT ( 'NONE',  ( -349.6046375497077179, 10.42115585936044830, 9.951701414186830458E-16 ) ) ;
#9928 = DIRECTION ( 'NONE',  ( -0.1566598588826321192, 0.9876526153536342445, 7.798540720466730171E-17 ) ) ;
#9929 = CIRCLE ( 'NONE', #11432, 1.499999999999999556 ) ;
#9930 = CARTESIAN_POINT ( 'NONE',  ( -57.69469991357523497, -24.33871690453385384, 4.330127018922218518 ) ) ;
#9931 = CARTESIAN_POINT ( 'NONE',  ( -65.10209452872746283, -25.51366584615358590, -8.660254037844380193 ) ) ;
#9932 = ADVANCED_FACE ( 'NONE', ( #11291 ), #7246, .F. ) ;
#9933 = B_SPLINE_CURVE_WITH_KNOTS ( 'NONE', 3,
 ( #12499, #18345, #2470, #5311, #768, #11065, #9675, #6837, #18240, #1153, #15535, #5501, #18337, #5212, #6544, #12289, #18129, #16694 ),
 .UNSPECIFIED., .F., .F.,
 ( 4, 2, 2, 2, 2, 2, 2, 2, 4 ),
 ( 0.000000000000000000, 0.0006036110467293980117, 0.001207222093458796023, 0.001810833140188194360, 0.002414444186917592047, 0.003018055233646990167, 0.003621666280376389154, 0.004225277327105789009, 0.004828888373835187563 ),
 .UNSPECIFIED. ) ;
#9934 = DIRECTION ( 'NONE',  ( 0.000000000000000000, 0.000000000000000000, 1.000000000000000000 ) ) ;
#9935 = AXIS2_PLACEMENT_3D ( 'NONE', #14040, #1089, #15272 ) ;
#9936 = LINE ( 'NONE', #15908, #12575 ) ;
#9937 = VECTOR ( 'NONE', #14584, 1000.000000000000000 ) ;
#9938 = DIRECTION ( 'NONE',  ( -0.9876526153536336894, -0.1566598588826349503, 0.000000000000000000 ) ) ;
#9939 = CYLINDRICAL_SURFACE ( 'NONE', #8727, 1.500000000000001554 ) ;
#9940 = DIRECTION ( 'NONE',  ( 0.000000000000000000, 0.000000000000000000, 1.000000000000000000 ) ) ;
#9941 = ORIENTED_EDGE ( 'NONE', *, *, #15550, .T. ) ;
#9942 = EDGE_LOOP ( 'NONE', ( #11630, #8797 ) ) ;
#9943 = DIRECTION ( 'NONE',  ( -0.1566598588826321192, 0.9876526153536342445, 7.798540720466730171E-17 ) ) ;
#9944 = ORIENTED_EDGE ( 'NONE', *, *, #14379, .T. ) ;
#9945 = VECTOR ( 'NONE', #3214, 1000.000000000000000 ) ;
#9946 = EDGE_LOOP ( 'NONE', ( #2602, #6999 ) ) ;
#9947 = EDGE_LOOP ( 'NONE', ( #13244, #1193 ) ) ;
#9948 = DIRECTION ( 'NONE',  ( -0.1566598588826321747, 0.9876526153536343555, 0.000000000000000000 ) ) ;
#9949 = CIRCLE ( 'NONE', #9046, 1.500000000000000444 ) ;
#9950 = FACE_OUTER_BOUND ( 'NONE', #215, .T. ) ;
#9951 = ADVANCED_FACE ( 'NONE', ( #17110 ), #660, .T. ) ;
#9952 = EDGE_CURVE ( 'NONE', #4233, #1545, #14902, .T. ) ;
#9953 = VERTEX_POINT ( 'NONE', #4468 ) ;
#9954 = CARTESIAN_POINT ( 'NONE',  ( -78.67338996650589422, 1.237145499066719001, -3.655658421838791750 ) ) ;
#9955 = ORIENTED_EDGE ( 'NONE', *, *, #9956, .T. ) ;
#9956 = EDGE_CURVE ( 'NONE', #17580, #16906, #39, .T. ) ;
#9957 = AXIS2_PLACEMENT_3D ( 'NONE', #13066, #10063, #11566 ) ;
#9958 = AXIS2_PLACEMENT_3D ( 'NONE', #5662, #15978, #1402 ) ;
#9959 = CARTESIAN_POINT ( 'NONE',  ( -49.59961335071796640, 35.00051552679456535, 20.00000000000001066 ) ) ;
#9960 = CARTESIAN_POINT ( 'NONE',  ( -63.78533391645962780, -88.07278042982854060, 8.660254037844412167 ) ) ;
#9961 = AXIS2_PLACEMENT_3D ( 'NONE', #154, #7450, #5659 ) ;
#9962 = AXIS2_PLACEMENT_3D ( 'NONE', #18116, #8326, #8133 ) ;
#9963 = AXIS2_PLACEMENT_3D ( 'NONE', #18579, #5545, #15206 ) ;
#9964 = DIRECTION ( 'NONE',  ( -0.9876526153536336894, -0.1566598588826349503, 0.000000000000000000 ) ) ;
#9965 = CYLINDRICAL_SURFACE ( 'NONE', #12686, 1.500000000000001554 ) ;
#9966 = DIRECTION ( 'NONE',  ( -0.1566598588826321192, 0.9876526153536342445, 7.798540720466730171E-17 ) ) ;
#9967 = VERTEX_POINT ( 'NONE', #13528 ) ;
#9968 = ORIENTED_EDGE ( 'NONE', *, *, #5442, .T. ) ;
#9969 = ORIENTED_EDGE ( 'NONE', *, *, #6124, .T. ) ;
#9970 = CIRCLE ( 'NONE', #17883, 1.499999999999999556 ) ;
#9971 = EDGE_LOOP ( 'NONE', ( #17016, #4124, #5937, #13112, #16656, #4786, #11026, #7680, #11544 ) ) ;
#9972 = DIRECTION ( 'NONE',  ( -0.9876526153536336894, -0.1566598588826349503, 0.000000000000000000 ) ) ;
#9973 = CIRCLE ( 'NONE', #5127, 1.500000000000000888 ) ;
#9974 = EDGE_LOOP ( 'NONE', ( #11448, #17174, #8618, #11040 ) ) ;
#9975 = CIRCLE ( 'NONE', #1807, 1.500000000000000888 ) ;
#9976 = ORIENTED_EDGE ( 'NONE', *, *, #7777, .F. ) ;
#9977 = DIRECTION ( 'NONE',  ( 0.9539392014169452150, -0.3000000000000013212, 0.000000000000000000 ) ) ;
#9978 = DIRECTION ( 'NONE',  ( -0.1566598588826321747, 0.9876526153536343555, 0.000000000000000000 ) ) ;
#9979 = VECTOR ( 'NONE', #15574, 1000.000000000000000 ) ;
#9980 = ADVANCED_FACE ( 'NONE', ( #7958 ), #578, .F. ) ;
#9981 = ADVANCED_FACE ( 'NONE', ( #16415, #11906 ), #17750, .T. ) ;
#9982 = CYLINDRICAL_SURFACE ( 'NONE', #11435, 144.0000000000000284 ) ;
#9983 = PRODUCT_CONTEXT ( 'NONE', #12312, 'mechanical' ) ;
#9984 = EDGE_CURVE ( 'NONE', #893, #16941, #16106, .T. ) ;
#9985 = AXIS2_PLACEMENT_3D ( 'NONE', #4512, #2996, #17259 ) ;
#9986 = FACE_OUTER_BOUND ( 'NONE', #6517, .T. ) ;
#9988 = DIRECTION ( 'NONE',  ( -0.000000000000000000, -0.000000000000000000, -1.000000000000000000 ) ) ;
#9987 = AXIS2_PLACEMENT_3D ( 'NONE', #11562, #14139, #2852 ) ;
#9989 = FACE_BOUND ( 'NONE', #3062, .T. ) ;
#9990 = CIRCLE ( 'NONE', #1543, 145.0000000000000284 ) ;
#9991 = VERTEX_POINT ( 'NONE', #7687 ) ;
#9992 = EDGE_LOOP ( 'NONE', ( #8188, #8845 ) ) ;
#9993 = CYLINDRICAL_SURFACE ( 'NONE', #6930, 1.500000000000001554 ) ;
#9994 = AXIS2_PLACEMENT_3D ( 'NONE', #11224, #11497, #14070 ) ;
#9995 = CARTESIAN_POINT ( 'NONE',  ( -46.33669483700848701, -22.53712852738358663, -4.330127018922180326 ) ) ;
#9996 = ORIENTED_EDGE ( 'NONE', *, *, #8342, .T. ) ;
#9997 = CARTESIAN_POINT ( 'NONE',  ( -64.31879523431432233, -30.45192892292171294, 1.869203119972154228E-14 ) ) ;
#9998 = VERTEX_POINT ( 'NONE', #18132 ) ;
#9999 = CIRCLE ( 'NONE', #31, 1.500000000000000888 ) ;
#10000 = CARTESIAN_POINT ( 'NONE',  ( -33.99103714508810725, -20.57888029135069985, 17.32050807568882078 ) ) ;
#10001 = AXIS2_PLACEMENT_3D ( 'NONE', #15983, #14569, #2822 ) ;
#10002 = DIRECTION ( 'NONE',  ( -0.1566598588826321192, 0.9876526153536342445, 7.798540720466730171E-17 ) ) ;
#10003 = CARTESIAN_POINT ( 'NONE',  ( -129.0554062880559627, 8.972188178592761076, 4.766626691765361912 ) ) ;
#10004 = AXIS2_PLACEMENT_3D ( 'NONE', #11318, #1399, #16077 ) ;
#10005 = DIRECTION ( 'NONE',  ( -0.1566598588826321747, 0.9876526153536343555, 0.000000000000000000 ) ) ;
#10006 = EDGE_CURVE ( 'NONE', #2561, #10528, #3389, .T. ) ;
#10007 = VECTOR ( 'NONE', #12636, 1000.000000000000000 ) ;
#10008 = EDGE_CURVE ( 'NONE', #18590, #4436, #9132, .T. ) ;
#10009 = CARTESIAN_POINT ( 'NONE',  ( -66.25446545484369665, -88.46443007703511796, 21.65063509461101532 ) ) ;
#10010 = DIRECTION ( 'NONE',  ( -0.1566598588826321192, 0.9876526153536342445, 7.798540720466730171E-17 ) ) ;
#10011 = VECTOR ( 'NONE', #11430, 1000.000000000000000 ) ;
#10012 = CARTESIAN_POINT ( 'NONE',  ( 0.000000000000000000, 0.000000000000000000, -20.00000000000000355 ) ) ;
#10013 = EDGE_LOOP ( 'NONE', ( #14493, #7575, #1728, #18208 ) ) ;
#10014 = DIRECTION ( 'NONE',  ( -0.9876526153536341335, -0.1566598588826330907, 0.000000000000000000 ) ) ;
#10015 = EDGE_CURVE ( 'NONE', #2063, #12573, #673, .T. ) ;
#10016 = AXIS2_PLACEMENT_3D ( 'NONE', #18391, #18089, #5364 ) ;
#10018 = VERTEX_POINT ( 'NONE', #1898 ) ;
#10017 = CARTESIAN_POINT ( 'NONE',  ( -29.05277406831996245, -19.79558099693753093, -17.32050807568878170 ) ) ;
#10019 = AXIS2_PLACEMENT_3D ( 'NONE', #905, #16740, #15284 ) ;
#10020 = LINE ( 'NONE', #15706, #11456 ) ;
#10021 = ORIENTED_EDGE ( 'NONE', *, *, #4969, .T. ) ;
#10022 = ORIENTED_EDGE ( 'NONE', *, *, #17340, .T. ) ;
#10023 = AXIS2_PLACEMENT_3D ( 'NONE', #17113, #9721, #15286 ) ;
#10024 = LINE ( 'NONE', #8334, #3356 ) ;
#10025 = VECTOR ( 'NONE', #16584, 1000.000000000000000 ) ;
#10026 = AXIS2_PLACEMENT_3D ( 'NONE', #8702, #14483, #14397 ) ;
#10027 = CYLINDRICAL_SURFACE ( 'NONE', #17928, 1.500000000000001554 ) ;
#10028 = CARTESIAN_POINT ( 'NONE',  ( -29.05277406831996245, -19.79558099693753448, 1.908195823574487804E-14 ) ) ;
#10029 = EDGE_LOOP ( 'NONE', ( #1949, #12922, #9922, #8206 ) ) ;
#10030 = FACE_OUTER_BOUND ( 'NONE', #11776, .T. ) ;
#10031 = PLANE ( 'NONE',  #10530 ) ;
#10032 = AXIS2_PLACEMENT_3D ( 'NONE', #8339, #5593, #9565 ) ;
#10033 = DIRECTION ( 'NONE',  ( -0.1566598588826321192, 0.9876526153536342445, 7.798540720466730171E-17 ) ) ;
#10034 = CARTESIAN_POINT ( 'NONE',  ( -10.98555400521827607, -21.99229654325962002, 21.65063509461101177 ) ) ;
#10035 = FACE_BOUND ( 'NONE', #3630, .T. ) ;
#10036 = CIRCLE ( 'NONE', #16716, 1.500000000000000000 ) ;
#10037 = EDGE_CURVE ( 'NONE', #18388, #411, #12105, .T. ) ;
#10038 = CARTESIAN_POINT ( 'NONE',  ( 3.000000000000000000, 0.000000000000000000, 37.00000000000000711 ) ) ;
#10039 = EDGE_LOOP ( 'NONE', ( #13703, #276, #12942, #16328, #7953, #11272 ) ) ;
#10040 = EDGE_LOOP ( 'NONE', ( #10725, #7170, #6144, #14362, #3027 ) ) ;
#10041 = DIRECTION ( 'NONE',  ( -0.9876526153536336894, -0.1566598588826349503, 0.000000000000000000 ) ) ;
#10042 = ORIENTED_EDGE ( 'NONE', *, *, #16638, .F. ) ;
#10043 = ORIENTED_EDGE ( 'NONE', *, *, #8382, .T. ) ;
#10044 = EDGE_CURVE ( 'NONE', #3838, #6198, #355, .T. ) ;
#10045 = EDGE_LOOP ( 'NONE', ( #8982, #17477, #12278, #4009 ) ) ;
#10046 = CYLINDRICAL_SURFACE ( 'NONE', #8963, 1.500000000000001554 ) ;
#10047 = AXIS2_PLACEMENT_3D ( 'NONE', #18713, #172, #17542 ) ;
#10048 = ADVANCED_FACE ( 'NONE', ( #764 ), #4993, .F. ) ;
#10049 = ORIENTED_EDGE ( 'NONE', *, *, #8465, .F. ) ;
#10050 = FACE_BOUND ( 'NONE', #8583, .T. ) ;
#10051 = LINE ( 'NONE', #11551, #16862 ) ;
#10052 = CARTESIAN_POINT ( 'NONE',  ( -79.05438463828195950, 1.499069270643396345, -3.389939594122236333 ) ) ;
#10053 = EDGE_LOOP ( 'NONE', ( #12894, #13726, #4350, #2384 ) ) ;
#10054 = TOROIDAL_SURFACE ( 'NONE', #13668, 3.000000000000000000, 2.000000000000000000 ) ;
#10055 = ORIENTED_EDGE ( 'NONE', *, *, #10944, .F. ) ;
#10056 =( GEOMETRIC_REPRESENTATION_CONTEXT ( 3 ) GLOBAL_UNCERTAINTY_ASSIGNED_CONTEXT ( ( #16130 ) ) GLOBAL_UNIT_ASSIGNED_CONTEXT ( ( #9497, #10988, #109 ) ) REPRESENTATION_CONTEXT ( 'NONE', 'WORKASPACE' ) );
#10057 = CARTESIAN_POINT ( 'NONE',  ( -9.464440072009985272, -79.45648819128378193, 17.32050807568880657 ) ) ;
#10058 = CIRCLE ( 'NONE', #7612, 1.500000000000000888 ) ;
#10059 = DIRECTION ( 'NONE',  ( -0.9876526153536341335, -0.1566598588826327021, 0.000000000000000000 ) ) ;
#10060 = DIRECTION ( 'NONE',  ( -0.1566598588826321192, 0.9876526153536342445, 7.798540720466731404E-17 ) ) ;
#10061 = CARTESIAN_POINT ( 'NONE',  ( -29.05277406831996245, -19.79558099693753448, 1.908195823574487804E-14 ) ) ;
#10062 = EDGE_CURVE ( 'NONE', #9117, #11762, #14872, .T. ) ;
#10063 = DIRECTION ( 'NONE',  ( -0.000000000000000000, -0.000000000000000000, -1.000000000000000000 ) ) ;
#10064 = EDGE_LOOP ( 'NONE', ( #9795, #13755 ) ) ;
#10065 = ADVANCED_FACE ( 'NONE', ( #10770 ), #13438, .F. ) ;
#10066 = ORIENTED_EDGE ( 'NONE', *, *, #12856, .F. ) ;
#10067 = VERTEX_POINT ( 'NONE', #16588 ) ;
#10068 = DIRECTION ( 'NONE',  ( -0.1566598588826321192, 0.9876526153536342445, 7.798540720466730171E-17 ) ) ;
#10069 = FACE_BOUND ( 'NONE', #15397, .T. ) ;
#10070 = FACE_OUTER_BOUND ( 'NONE', #10165, .T. ) ;
#10071 = ORIENTED_EDGE ( 'NONE', *, *, #6271, .F. ) ;
#10072 = DIRECTION ( 'NONE',  ( -0.9876526153536336894, -0.1566598588826349503, 0.000000000000000000 ) ) ;
#10073 = DIRECTION ( 'NONE',  ( -0.1566598588826321192, 0.9876526153536342445, 7.798540720466730171E-17 ) ) ;
#10074 = CARTESIAN_POINT ( 'NONE',  ( -77.18258565727082043, 4.450738551673800281, 20.00000000000000711 ) ) ;
#10075 = ITEM_DEFINED_TRANSFORMATION ( 'NONE', 'NONE', #837,  #18772 ) ;
#10076 = ORIENTED_EDGE ( 'NONE', *, *, #10044, .T. ) ;
#10077 = EDGE_CURVE ( 'NONE', #4362, #8991, #3077, .T. ) ;
#10078 = DIRECTION ( 'NONE',  ( -0.1566598588826321192, 0.9876526153536342445, 7.798540720466731404E-17 ) ) ;
#10079 = DIRECTION ( 'NONE',  ( -0.1566598588826321747, 0.9876526153536343555, 0.000000000000000000 ) ) ;
#10080 = ADVANCED_FACE ( 'NONE', ( #9277 ), #6463, .F. ) ;
#10081 = CARTESIAN_POINT ( 'NONE',  ( -70.00000000000001421, 44.99999999999997868, -7.169095027853613189 ) ) ;
#10082 = EDGE_CURVE ( 'NONE', #3359, #7684, #3659, .T. ) ;
#10083 = VERTEX_POINT ( 'NONE', #14967 ) ;
#10084 = ORIENTED_EDGE ( 'NONE', *, *, #11096, .T. ) ;
#10085 = CIRCLE ( 'NONE', #4640, 1.500000000000001332 ) ;
#10086 = CARTESIAN_POINT ( 'NONE',  ( -20.16390053013728334, -18.38564226699384818, -12.99038105676658006 ) ) ;
#10087 = EDGE_CURVE ( 'NONE', #9184, #13174, #4287, .T. ) ;
#10088 = DIRECTION ( 'NONE',  ( 1.000000000000000000, 0.000000000000000000, 0.000000000000000000 ) ) ;
#10089 = DIRECTION ( 'NONE',  ( 1.000000000000000000, 0.000000000000000000, 0.000000000000000000 ) ) ;
#10090 = FACE_OUTER_BOUND ( 'NONE', #4769, .T. ) ;
#10091 = VERTEX_POINT ( 'NONE', #15059 ) ;
#10092 = EDGE_LOOP ( 'NONE', ( #7795, #5014 ) ) ;
#10093 = CARTESIAN_POINT ( 'NONE',  ( -77.72973689007648090, 30.96463005215034059, -35.00000000000000000 ) ) ;
#10094 = CIRCLE ( 'NONE', #1931, 1.500000000000000888 ) ;
#10095 = DIRECTION ( 'NONE',  ( -0.9876526153536341335, -0.1566598588826327021, 0.000000000000000000 ) ) ;
#10096 = LINE ( 'NONE', #17423, #607 ) ;
#10097 = CYLINDRICAL_SURFACE ( 'NONE', #14806, 1.500000000000001554 ) ;
#10098 =( LENGTH_UNIT ( ) NAMED_UNIT ( * ) SI_UNIT ( .MILLI., .METRE. ) );
#10099 = DIRECTION ( 'NONE',  ( -0.9876526153536341335, -0.1566598588826327021, 0.000000000000000000 ) ) ;
#10100 = LINE ( 'NONE', #1322, #17161 ) ;
#10101 = DIRECTION ( 'NONE',  ( 1.000000000000000000, 0.000000000000000000, 0.000000000000000000 ) ) ;
#10102 = EDGE_LOOP ( 'NONE', ( #11758, #3377, #13984, #12758 ) ) ;
#10103 = CARTESIAN_POINT ( 'NONE',  ( -30.73860631229088725, -25.12549372091224598, 21.65063509461101887 ) ) ;
#10104 = EDGE_LOOP ( 'NONE', ( #327, #672, #3431, #17260 ) ) ;
#10106 = ORIENTED_EDGE ( 'NONE', *, *, #16598, .T. ) ;
#10105 = CARTESIAN_POINT ( 'NONE',  ( -29.25712738926043244, -24.89050393258829175, 12.99038105676661736 ) ) ;
#10107 = ORIENTED_EDGE ( 'NONE', *, *, #11352, .T. ) ;
#10108 = FACE_OUTER_BOUND ( 'NONE', #11249, .T. ) ;
#10109 = DIRECTION ( 'NONE',  ( -0.9876526153536341335, -0.1566598588826327021, 0.000000000000000000 ) ) ;
#10110 = ORIENTED_EDGE ( 'NONE', *, *, #13501, .F. ) ;
#10111 = ADVANCED_FACE ( 'NONE', ( #6932 ), #12669, .F. ) ;
#10112 = EDGE_CURVE ( 'NONE', #13905, #3440, #7931, .T. ) ;
#10113 = CARTESIAN_POINT ( 'NONE',  ( -55.42992169613163611, -29.04199019297804085, -12.99038105676658006 ) ) ;
#10114 = DIRECTION ( 'NONE',  ( 0.000000000000000000, -1.000000000000000000, 0.000000000000000000 ) ) ;
#10115 = FACE_OUTER_BOUND ( 'NONE', #632, .T. ) ;
#10116 = VERTEX_POINT ( 'NONE', #9930 ) ;
#10117 = DIRECTION ( 'NONE',  ( -0.9876526153536336894, -0.1566598588826349503, 0.000000000000000000 ) ) ;
#10118 = LINE ( 'NONE', #4616, #14586 ) ;
#10119 = DIRECTION ( 'NONE',  ( -0.1566598588826321747, 0.9876526153536343555, 0.000000000000000000 ) ) ;
#10120 = DIRECTION ( 'NONE',  ( -0.1566598588826321192, 0.9876526153536342445, 7.798540720466730171E-17 ) ) ;
#10121 = EDGE_LOOP ( 'NONE', ( #11691, #3134, #6215, #1888 ) ) ;
#10122 = CARTESIAN_POINT ( 'NONE',  ( -10.94591899504043830, -79.69147797960773971, 8.660254037844412167 ) ) ;
#10123 = CARTESIAN_POINT ( 'NONE',  ( -63.82496892663746735, -30.37359899348040315, 4.330127018922217630 ) ) ;
#10124 = DIRECTION ( 'NONE',  ( -0.1566598588826321192, 0.9876526153536342445, 7.798540720466731404E-17 ) ) ;
#10125 = EDGE_LOOP ( 'NONE', ( #6821, #180, #11340, #4628 ) ) ;
#10126 = ORIENTED_EDGE ( 'NONE', *, *, #16699, .T. ) ;
#10127 = VERTEX_POINT ( 'NONE', #10968 ) ;
#10128 = CARTESIAN_POINT ( 'NONE',  ( -6.047290928450125946, -21.20899724884646531, -21.65063509461098334 ) ) ;
#10129 = ORIENTED_EDGE ( 'NONE', *, *, #15869, .F. ) ;
#10130 = LINE ( 'NONE', #8843, #18392 ) ;
#10131 = ORIENTED_EDGE ( 'NONE', *, *, #13938, .F. ) ;
#10132 = CARTESIAN_POINT ( 'NONE',  ( -15.92381708198643153, -22.77559583767277473, 12.99038105676661381 ) ) ;
#10133 = ADVANCED_FACE ( 'NONE', ( #15720 ), #16799, .F. ) ;
#10134 = DIRECTION ( 'NONE',  ( 0.000000000000000000, 0.000000000000000000, 1.000000000000000000 ) ) ;
#10135 = ADVANCED_FACE ( 'NONE', ( #4143 ), #17078, .F. ) ;
#10136 = DIRECTION ( 'NONE',  ( -0.1566598588826321192, 0.9876526153536342445, 7.798540720466731404E-17 ) ) ;
#10137 = AXIS2_PLACEMENT_3D ( 'NONE', #5456, #12458, #7085 ) ;
#10138 = LINE ( 'NONE', #2934, #2981 ) ;
#10139 = EDGE_LOOP ( 'NONE', ( #5517, #6119 ) ) ;
#10140 = EDGE_CURVE ( 'NONE', #3470, #4130, #3759, .T. ) ;
#10141 = DIRECTION ( 'NONE',  ( 0.000000000000000000, 0.000000000000000000, -1.000000000000000000 ) ) ;
#10142 =( REPRESENTATION_RELATIONSHIP ('NONE','NONE', #7353, #6739 ) REPRESENTATION_RELATIONSHIP_WITH_TRANSFORMATION ( #12621 )SHAPE_REPRESENTATION_RELATIONSHIP( ) );
#10143 = CARTESIAN_POINT ( 'NONE',  ( 0.000000000000000000, 0.000000000000000000, -30.00000000000000000 ) ) ;
#10144 = CYLINDRICAL_SURFACE ( 'NONE', #16347, 1.500000000000001554 ) ;
#10145 = DIRECTION ( 'NONE',  ( -0.9876526153536336894, -0.1566598588826349503, 0.000000000000000000 ) ) ;
#10146 = CARTESIAN_POINT ( 'NONE',  ( -78.43540483600145308, -27.62857394106911357, -8.660254037844380193 ) ) ;
#10147 = AXIS2_PLACEMENT_3D ( 'NONE', #5140, #15273, #8282 ) ;
#10148 = ORIENTED_EDGE ( 'NONE', *, *, #2033, .F. ) ;
#10149 = EDGE_LOOP ( 'NONE', ( #5370, #18325 ) ) ;
#10150 = VERTEX_POINT ( 'NONE', #2464 ) ;
#10151 = CARTESIAN_POINT ( 'NONE',  ( -4.565812005419673802, -20.97400746052251108, -12.99038105676658006 ) ) ;
#10152 = ORIENTED_EDGE ( 'NONE', *, *, #13875, .F. ) ;
#10153 = FACE_OUTER_BOUND ( 'NONE', #1677, .T. ) ;
#10154 = DIRECTION ( 'NONE',  ( 1.000000000000000000, 0.000000000000000000, -2.631994239413086031E-16 ) ) ;
#10155 = ORIENTED_EDGE ( 'NONE', *, *, #5692, .F. ) ;
#10156 = VECTOR ( 'NONE', #14983, 1000.000000000000000 ) ;
#10157 = EDGE_CURVE ( 'NONE', #4419, #16131, #11532, .T. ) ;
#10158 = AXIS2_PLACEMENT_3D ( 'NONE', #6648, #11066, #15250 ) ;
#10159 = CARTESIAN_POINT ( 'NONE',  ( -49.59961335071797350, 37.20051552679458240, -130.3485206753969976 ) ) ;
#10160 = LINE ( 'NONE', #17594, #6725 ) ;
#10161 = EDGE_CURVE ( 'NONE', #15907, #491, #3363, .T. ) ;
#10162 = CARTESIAN_POINT ( 'NONE',  ( -174.8823813673296286, 55.30280195509305230, 5.132545408516865137 ) ) ;
#10163 = DIRECTION ( 'NONE',  ( -1.000000000000000000, 0.000000000000000000, 0.000000000000000000 ) ) ;
#10164 = PLANE ( 'NONE',  #6234 ) ;
#10165 = EDGE_LOOP ( 'NONE', ( #13480, #12153, #4739, #5987 ) ) ;
#10166 = ORIENTED_EDGE ( 'NONE', *, *, #7613, .T. ) ;
#10167 = LINE ( 'NONE', #12917, #12650 ) ;
#10168 = AXIS2_PLACEMENT_3D ( 'NONE', #13646, #12308, #12212 ) ;
#10169 = DIRECTION ( 'NONE',  ( -0.1566598588826321192, 0.9876526153536342445, 7.798540720466731404E-17 ) ) ;
#10170 = AXIS2_PLACEMENT_3D ( 'NONE', #15426, #2446, #4029 ) ;
#10171 = VERTEX_POINT ( 'NONE', #5399 ) ;
#10172 = DIRECTION ( 'NONE',  ( -0.1566598588826321192, 0.9876526153536342445, 7.798540720466730171E-17 ) ) ;
#10173 = EDGE_CURVE ( 'NONE', #10331, #14323, #10327, .T. ) ;
#10174 = AXIS2_PLACEMENT_3D ( 'NONE', #7574, #13237, #376 ) ;
#10175 = EDGE_CURVE ( 'NONE', #12283, #5678, #2163, .T. ) ;
#10176 = DIRECTION ( 'NONE',  ( 0.000000000000000000, 0.000000000000000000, 1.000000000000000000 ) ) ;
#10177 = EDGE_CURVE ( 'NONE', #12874, #14890, #9847, .T. ) ;
#10178 = CIRCLE ( 'NONE', #5961, 1.499999999999999556 ) ;
#10179 = DIRECTION ( 'NONE',  ( -0.1566598588826321192, 0.9876526153536342445, 7.798540720466731404E-17 ) ) ;
#10180 =( NAMED_UNIT ( * ) PLANE_ANGLE_UNIT ( ) SI_UNIT ( $, .RADIAN. ) );
#10181 = ADVANCED_FACE ( 'NONE', ( #15536 ), #5306, .T. ) ;
#10182 = ADVANCED_FACE ( 'NONE', ( #8430 ), #2550, .F. ) ;
#10183 = CARTESIAN_POINT ( 'NONE',  ( -129.1404785418517918, -2.850701963179328668, 9.951701414186818625E-16 ) ) ;
#10184 = AXIS2_PLACEMENT_3D ( 'NONE', #18293, #5263, #15497 ) ;
#10185 = DIRECTION ( 'NONE',  ( -0.1566598588826321192, 0.9876526153536342445, 7.798540720466730171E-17 ) ) ;
#10186 = VECTOR ( 'NONE', #17415, 1000.000000000000114 ) ;
#10187 = CARTESIAN_POINT ( 'NONE',  ( -2.000000000000000000, 2.449293598294706414E-16, -20.00000000000000355 ) ) ;
#10188 = CARTESIAN_POINT ( 'NONE',  ( -73.70149508017377116, -31.94019758230671258, 21.65063509461101887 ) ) ;
#10189 = ORIENTED_EDGE ( 'NONE', *, *, #10112, .T. ) ;
#10190 = CARTESIAN_POINT ( 'NONE',  ( 0.000000000000000000, 0.000000000000000000, -25.65685424949237614 ) ) ;
#10191 = AXIS2_PLACEMENT_3D ( 'NONE', #17814, #10476, #14751 ) ;
#10192 = VERTEX_POINT ( 'NONE', #14104 ) ;
#10193 = ORIENTED_EDGE ( 'NONE', *, *, #12296, .F. ) ;
#10194 = AXIS2_PLACEMENT_3D ( 'NONE', #10646, #3863, #14909 ) ;
#10195 = ORIENTED_EDGE ( 'NONE', *, *, #17862, .F. ) ;
#10196 = EDGE_LOOP ( 'NONE', ( #16591, #7672 ) ) ;
#10197 = ORIENTED_EDGE ( 'NONE', *, *, #15308, .F. ) ;
#10198 = STYLED_ITEM ( 'NONE', ( #12753 ), #9123 ) ;
#10199 = CARTESIAN_POINT ( 'NONE',  ( -2.000000000000000000, 0.000000000000000000, 24.99999999999999289 ) ) ;
#10200 = CIRCLE ( 'NONE', #4455, 1.499999999999999556 ) ;
#10201 = EDGE_LOOP ( 'NONE', ( #8035, #7382, #15586, #680 ) ) ;
#10202 = ADVANCED_FACE ( 'NONE', ( #1155 ), #14207, .F. ) ;
#10203 = CARTESIAN_POINT ( 'NONE',  ( -11.97320662057189899, -22.14895640214223960, 8.660254037844413944 ) ) ;
#10204 = DIRECTION ( 'NONE',  ( -1.000000000000000000, 0.000000000000000000, 0.000000000000000000 ) ) ;
#10205 = DIRECTION ( 'NONE',  ( 8.693966348389027220E-17, -1.991237296706374949E-16, 1.000000000000000000 ) ) ;
#10206 = DIRECTION ( 'NONE',  ( -0.1566598588826321192, 0.9876526153536342445, 7.798540720466730171E-17 ) ) ;
#10207 = CARTESIAN_POINT ( 'NONE',  ( -3.044698072211382112, -78.43819910854666944, 1.443110928631665584E-14 ) ) ;
#10208 = AXIS2_PLACEMENT_3D ( 'NONE', #1928, #13468, #6208 ) ;
#10209 = EDGE_CURVE ( 'NONE', #4467, #93, #1865, .T. ) ;
#10210 = DIRECTION ( 'NONE',  ( -1.000000000000000000, 0.000000000000000000, 0.000000000000000000 ) ) ;
#10211 = ORIENTED_EDGE ( 'NONE', *, *, #11227, .T. ) ;
#10213 = EDGE_CURVE ( 'NONE', #5894, #12413, #8235, .T. ) ;
#10212 = DIRECTION ( 'NONE',  ( 0.000000000000000000, 0.000000000000000000, 1.000000000000000000 ) ) ;
#10214 = EDGE_CURVE ( 'NONE', #12208, #13656, #3974, .T. ) ;
#10215 = EDGE_CURVE ( 'NONE', #4978, #1633, #10118, .T. ) ;
#10216 = CYLINDRICAL_SURFACE ( 'NONE', #1178, 1.500000000000001554 ) ;
#10217 = DIRECTION ( 'NONE',  ( -1.000000000000000000, 0.000000000000000000, 0.000000000000000000 ) ) ;
#10218 = PRODUCT_DEFINITION_FORMATION_WITH_SPECIFIED_SOURCE ( 'ANY', '', #2590, .NOT_KNOWN. ) ;
#10220 = ORIENTED_EDGE ( 'NONE', *, *, #15412, .F. ) ;
#10219 = CARTESIAN_POINT ( 'NONE',  ( -28.26947477390680774, -24.73384407370567217, 17.32050807568881723 ) ) ;
#10221 = ORIENTED_EDGE ( 'NONE', *, *, #8342, .F. ) ;
#10222 = CARTESIAN_POINT ( 'NONE',  ( 2.200000000000000178, 2.694222958124177006E-16, 25.00000000000000000 ) ) ;
#10223 = ORIENTED_EDGE ( 'NONE', *, *, #5923, .F. ) ;
#10224 = VERTEX_POINT ( 'NONE', #6056 ) ;
#10225 = CARTESIAN_POINT ( 'NONE',  ( -6.830590222863280658, -16.27073417207831696, -4.330127018922183879 ) ) ;
#10226 = CIRCLE ( 'NONE', #2056, 150.0000000000000000 ) ;
#10227 = ORIENTED_EDGE ( 'NONE', *, *, #15847, .F. ) ;
#10228 = FACE_BOUND ( 'NONE', #12556, .T. ) ;
#10229 = VERTEX_POINT ( 'NONE', #11799 ) ;
#10230 = AXIS2_PLACEMENT_3D ( 'NONE', #8047, #9379, #479 ) ;
#10231 = DIRECTION ( 'NONE',  ( -0.1566598588826321747, 0.9876526153536343555, 0.000000000000000000 ) ) ;
#10232 = UNCERTAINTY_MEASURE_WITH_UNIT (LENGTH_MEASURE( 1.000000000000000082E-05 ), #18607, 'distance_accuracy_value', 'NONE');
#10233 = CARTESIAN_POINT ( 'NONE',  ( -11.97320662057189899, -22.14895640214223960, -8.660254037844380193 ) ) ;
#10234 = CARTESIAN_POINT ( 'NONE',  ( -27.57129514528951120, -19.56059120861358380, -17.32050807568878170 ) ) ;
#10235 = ORIENTED_EDGE ( 'NONE', *, *, #2532, .T. ) ;
#10236 = ADVANCED_FACE ( 'NONE', ( #2047 ), #11617, .F. ) ;
#10237 = ORIENTED_EDGE ( 'NONE', *, *, #16457, .F. ) ;
#10238 = EDGE_CURVE ( 'NONE', #8901, #4830, #8969, .T. ) ;
#10239 = CARTESIAN_POINT ( 'NONE',  ( -71.23236354178970942, -31.54854793510013877, 8.660254037844417496 ) ) ;
#10240 = LINE ( 'NONE', #17826, #2433 ) ;
#10241 = DIRECTION ( 'NONE',  ( -1.000000000000000000, 0.000000000000000000, 0.000000000000000000 ) ) ;
#10242 = AXIS2_PLACEMENT_3D ( 'NONE', #92, #1613, #7475 ) ;
#10243 = CARTESIAN_POINT ( 'NONE',  ( -67.77557938805200877, -31.00023842901093118, 17.32050807568881723 ) ) ;
#10244 = EDGE_CURVE ( 'NONE', #2879, #1265, #9429, .T. ) ;
#10245 = VECTOR ( 'NONE', #8180, 1000.000000000000000 ) ;
#10246 = ORIENTED_EDGE ( 'NONE', *, *, #15525, .T. ) ;
#10247 = VERTEX_POINT ( 'NONE', #5790 ) ;
#10248 = VERTEX_POINT ( 'NONE', #1610 ) ;
#10249 = DIRECTION ( 'NONE',  ( 1.000000000000000000, 0.000000000000000000, 0.000000000000000000 ) ) ;
#10250 = ORIENTED_EDGE ( 'NONE', *, *, #16123, .T. ) ;
#10251 = FACE_BOUND ( 'NONE', #642, .T. ) ;
#10252 = CIRCLE ( 'NONE', #1493, 2.000000000000001776 ) ;
#10253 = DIRECTION ( 'NONE',  ( -0.1566598588826321192, 0.9876526153536342445, 7.798540720466730171E-17 ) ) ;
#10254 = EDGE_LOOP ( 'NONE', ( #14866, #8029, #9422, #10319 ) ) ;
#10255 = CARTESIAN_POINT ( 'NONE',  ( -10.98555400521827963, -21.99229654325962002, -21.65063509461098334 ) ) ;
#10256 = CIRCLE ( 'NONE', #6946, 1.499999999999999556 ) ;
#10257 = VERTEX_POINT ( 'NONE', #14487 ) ;
#10258 = CIRCLE ( 'NONE', #4814, 1.500000000000000888 ) ;
#10259 = AXIS2_PLACEMENT_3D ( 'NONE', #11984, #17827, #11710 ) ;
#10260 = ORIENTED_EDGE ( 'NONE', *, *, #10990, .F. ) ;
#10261 = DIRECTION ( 'NONE',  ( -0.9876526153536341335, -0.1566598588826327021, 0.000000000000000000 ) ) ;
#10262 = CARTESIAN_POINT ( 'NONE',  ( -174.3165826136136332, 55.97625804580273012, 3.566331213966862368 ) ) ;
#10263 = CYLINDRICAL_SURFACE ( 'NONE', #11761, 2.200000000000000622 ) ;
#10264 = CARTESIAN_POINT ( 'NONE',  ( -174.8433004229789844, 55.46678263321123126, -4.764204982952879419 ) ) ;
#10265 = DIRECTION ( 'NONE',  ( -0.7999937637212570785, 0.6000083149482993150, -7.754303923936027931E-17 ) ) ;
#10266 = EDGE_LOOP ( 'NONE', ( #7417, #6705, #18368, #18268 ) ) ;
#10267 = EDGE_LOOP ( 'NONE', ( #16945, #14984 ) ) ;
#10268 = CYLINDRICAL_SURFACE ( 'NONE', #2970, 2.200000000000000178 ) ;
#10269 = ADVANCED_FACE ( 'NONE', ( #17272 ), #7121, .F. ) ;
#10270 = DIRECTION ( 'NONE',  ( -0.1566598588826321192, 0.9876526153536342445, 7.798540720466730171E-17 ) ) ;
#10271 = CARTESIAN_POINT ( 'NONE',  ( -38.92930022185626626, -21.36217958576384390, -17.32050807568878170 ) ) ;
#10272 = AXIS2_PLACEMENT_3D ( 'NONE', #5167, #10930, #3721 ) ;
#10273 = CIRCLE ( 'NONE', #2959, 1.500000000000000000 ) ;
#10274 = AXIS2_PLACEMENT_3D ( 'NONE', #10159, #13919, #7771 ) ;
#10275 = ORIENTED_EDGE ( 'NONE', *, *, #5975, .T. ) ;
#10276 = CARTESIAN_POINT ( 'NONE',  ( -79.30363509306917535, 32.43333333333333002, 92.77853496600735639 ) ) ;
#10277 = EDGE_CURVE ( 'NONE', #7186, #14747, #3010, .T. ) ;
#10278 = CIRCLE ( 'NONE', #2112, 1.500000000000000888 ) ;
#10279 = DIRECTION ( 'NONE',  ( -0.9876526153536336894, -0.1566598588826349503, 0.000000000000000000 ) ) ;
#10280 = AXIS2_PLACEMENT_3D ( 'NONE', #9306, #15190, #13948 ) ;
#10281 = CARTESIAN_POINT ( 'NONE',  ( -69.99999999999998579, -45.00000000000000711, -19.99999999999999645 ) ) ;
#10282 = CYLINDRICAL_SURFACE ( 'NONE', #17217, 2.000000000000000000 ) ;
#10283 =( NAMED_UNIT ( * ) SI_UNIT ( $, .STERADIAN. ) SOLID_ANGLE_UNIT ( ) );
#10284 = CIRCLE ( 'NONE', #14538, 2.500000000000002220 ) ;
#10285 = CARTESIAN_POINT ( 'NONE',  ( -6.007655918272284623, -78.90817868519457079, -8.660254037844385522 ) ) ;
#10286 = CIRCLE ( 'NONE', #7568, 1.500000000000001332 ) ;
#10287 = LINE ( 'NONE', #1592, #8375 ) ;
#10288 = CYLINDRICAL_SURFACE ( 'NONE', #10433, 1.500000000000001554 ) ;
#10289 = FACE_OUTER_BOUND ( 'NONE', #13591, .T. ) ;
#10290 = VERTEX_POINT ( 'NONE', #12866 ) ;
#10291 = VERTEX_POINT ( 'NONE', #10306 ) ;
#10292 = DIRECTION ( 'NONE',  ( 2.671473304378624222E-16, 0.000000000000000000, 1.000000000000000000 ) ) ;
#10293 = ORIENTED_EDGE ( 'NONE', *, *, #4439, .T. ) ;
#10294 = CIRCLE ( 'NONE', #4837, 1.500000000000000888 ) ;
#10295 = EDGE_CURVE ( 'NONE', #8550, #8304, #17361, .T. ) ;
#10296 = EDGE_CURVE ( 'NONE', #16997, #4463, #13369, .T. ) ;
#10297 = DIRECTION ( 'NONE',  ( -0.1566598588826321192, 0.9876526153536342445, 7.798540720466730171E-17 ) ) ;
#10298 = AXIS2_PLACEMENT_3D ( 'NONE', #7853, #13616, #14617 ) ;
#10299 = VERTEX_POINT ( 'NONE', #7472 ) ;
#10300 = EDGE_CURVE ( 'NONE', #11204, #16695, #11433, .T. ) ;
#10301 = DIRECTION ( 'NONE',  ( 1.000000000000000000, 0.000000000000000000, 0.000000000000000000 ) ) ;
#10302 = AXIS2_PLACEMENT_3D ( 'NONE', #8398, #8502, #12841 ) ;
#10303 = LINE ( 'NONE', #11797, #15791 ) ;
#10304 = DIRECTION ( 'NONE',  ( 1.000000000000000000, 0.000000000000000000, 0.000000000000000000 ) ) ;
#10305 = DIRECTION ( 'NONE',  ( -1.000000000000000000, 0.000000000000000000, 0.000000000000000000 ) ) ;
#10306 = CARTESIAN_POINT ( 'NONE',  ( -76.88766983611584749, -2.536636612185957595, 7.500000000000000000 ) ) ;
#10307 = CYLINDRICAL_SURFACE ( 'NONE', #11440, 1.500000000000001554 ) ;
#10308 = AXIS2_PLACEMENT_3D ( 'NONE', #14080, #8400, #15800 ) ;
#10309 = DIRECTION ( 'NONE',  ( -0.9876526153536336894, -0.1566598588826349503, 0.000000000000000000 ) ) ;
#10310 = VECTOR ( 'NONE', #14658, 1000.000000000000000 ) ;
#10311 = DIRECTION ( 'NONE',  ( -0.1566598588826321192, 0.9876526153536342445, 7.798540720466730171E-17 ) ) ;
#10312 = DIRECTION ( 'NONE',  ( -0.1566598588826321747, 0.9876526153536343555, 0.000000000000000000 ) ) ;
#10313 = CARTESIAN_POINT ( 'NONE',  ( 0.000000000000000000, 0.000000000000000000, -20.00000000000000355 ) ) ;
#10314 = EDGE_CURVE ( 'NONE', #10907, #3313, #15188, .T. ) ;
#10315 = ADVANCED_FACE ( 'NONE', ( #4346 ), #89, .F. ) ;
#10316 = EDGE_LOOP ( 'NONE', ( #14677, #474 ) ) ;
#10317 = VECTOR ( 'NONE', #10553, 1000.000000000000000 ) ;
#10319 = ORIENTED_EDGE ( 'NONE', *, *, #9011, .F. ) ;
#10318 = ADVANCED_FACE ( 'NONE', ( #14583 ), #11704, .F. ) ;
#10320 = DIRECTION ( 'NONE',  ( 0.000000000000000000, 0.000000000000000000, 1.000000000000000000 ) ) ;
#10321 = EDGE_LOOP ( 'NONE', ( #15581, #9085 ) ) ;
#10322 = ORIENTED_EDGE ( 'NONE', *, *, #2532, .F. ) ;
#10323 = VECTOR ( 'NONE', #10386, 1000.000000000000227 ) ;
#10324 = FACE_OUTER_BOUND ( 'NONE', #1657, .T. ) ;
#10325 = DIRECTION ( 'NONE',  ( -0.9876526153536336894, -0.1566598588826349503, 0.000000000000000000 ) ) ;
#10326 = VERTEX_POINT ( 'NONE', #4525 ) ;
#10327 = CIRCLE ( 'NONE', #2482, 1.500000000000001332 ) ;
#10328 = CARTESIAN_POINT ( 'NONE',  ( -40.61513246582718040, -26.69209230973856251, 21.65063509461101887 ) ) ;
#10329 = VERTEX_POINT ( 'NONE', #17647 ) ;
#10330 = AXIS2_PLACEMENT_3D ( 'NONE', #16150, #1729, #7517 ) ;
#10331 = VERTEX_POINT ( 'NONE', #16103 ) ;
#10332 = DIRECTION ( 'NONE',  ( -0.1566598588826321747, 0.9876526153536343555, 0.000000000000000000 ) ) ;
#10333 = DIRECTION ( 'NONE',  ( -0.9876526153536341335, -0.1566598588826327021, 0.000000000000000000 ) ) ;
#10334 = CARTESIAN_POINT ( 'NONE',  ( -35.67686938905902849, -25.90879301532540779, 4.330127018922217630 ) ) ;
#10335 = AXIS2_PLACEMENT_3D ( 'NONE', #1686, #13233, #10391 ) ;
#10336 = ORIENTED_EDGE ( 'NONE', *, *, #7448, .T. ) ;
#10337 = EDGE_LOOP ( 'NONE', ( #17008, #2827, #5773, #11985, #8335 ) ) ;
#10338 = ORIENTED_EDGE ( 'NONE', *, *, #3193, .T. ) ;
#10339 = FACE_OUTER_BOUND ( 'NONE', #2950, .T. ) ;
#10340 = VERTEX_POINT ( 'NONE', #4251 ) ;
#10341 = VERTEX_POINT ( 'NONE', #3100 ) ;
#10342 = FACE_BOUND ( 'NONE', #2677, .T. ) ;
#10343 = ADVANCED_FACE ( 'NONE', ( #10030 ), #14669, .F. ) ;
#10344 = CIRCLE ( 'NONE', #14305, 20.00000000000001066 ) ;
#10345 = DIRECTION ( 'NONE',  ( -1.000000000000000000, 0.000000000000000000, 0.000000000000000000 ) ) ;
#10346 = ADVANCED_FACE ( 'NONE', ( #16190 ), #10480, .F. ) ;
#10347 = ORIENTED_EDGE ( 'NONE', *, *, #17752, .T. ) ;
#10348 = CARTESIAN_POINT ( 'NONE',  ( -54.44226908077801852, -28.88533033409541062, -17.32050807568878170 ) ) ;
#10349 = ORIENTED_EDGE ( 'NONE', *, *, #15638, .F. ) ;
#10350 = VECTOR ( 'NONE', #17727, 1000.000000000000000 ) ;
#10351 = EDGE_CURVE ( 'NONE', #14703, #16242, #9075, .T. ) ;
#10352 = VERTEX_POINT ( 'NONE', #13504 ) ;
#10353 = CARTESIAN_POINT ( 'NONE',  ( -19.87442754340095519, -23.40223527320329922, -17.32050807568878170 ) ) ;
#10354 = DIRECTION ( 'NONE',  ( -0.000000000000000000, -0.000000000000000000, -1.000000000000000000 ) ) ;
#10355 = DIRECTION ( 'NONE',  ( 0.9868632313631133801, 0.1615579233078775490, -2.699728182682516797E-16 ) ) ;
#10356 = DIRECTION ( 'NONE',  ( -0.1566598588826321192, 0.9876526153536342445, 7.798540720466731404E-17 ) ) ;
#10357 = LINE ( 'NONE', #8858, #10538 ) ;
#10358 = CARTESIAN_POINT ( 'NONE',  ( 8.807133312032172867, -76.55828080195509244, 17.32050807568880657 ) ) ;
#10359 = ORIENTED_EDGE ( 'NONE', *, *, #148, .F. ) ;
#10360 = ORIENTED_EDGE ( 'NONE', *, *, #14331, .T. ) ;
#10361 = DIRECTION ( 'NONE',  ( -0.1566598588826321192, 0.9876526153536342445, 7.798540720466730171E-17 ) ) ;
#10362 = CARTESIAN_POINT ( 'NONE',  ( -20.82244514857674389, -81.25807656843404914, -17.32050807568878525 ) ) ;
#10363 = CARTESIAN_POINT ( 'NONE',  ( -172.7326993491721225, 43.83249341393818810, 9.951701414186830458E-16 ) ) ;
#10364 = CIRCLE ( 'NONE', #12796, 1.500000000000001332 ) ;
#10365 = ORIENTED_EDGE ( 'NONE', *, *, #10987, .F. ) ;
#10366 = DIRECTION ( 'NONE',  ( -0.000000000000000000, -0.000000000000000000, -1.000000000000000000 ) ) ;
#10367 = FACE_BOUND ( 'NONE', #11637, .T. ) ;
#10368 = CARTESIAN_POINT ( 'NONE',  ( -27.73601345605214519, -82.35469558061247142, -17.32050807568878525 ) ) ;
#10369 = ADVANCED_FACE ( 'NONE', ( #16275 ), #17926, .F. ) ;
#10370 = PLANE ( 'NONE',  #7863 ) ;
#10371 = DIRECTION ( 'NONE',  ( -0.1566598588826321192, 0.9876526153536342445, 7.798540720466730171E-17 ) ) ;
#10372 = VERTEX_POINT ( 'NONE', #5073 ) ;
#10373 = AXIS2_PLACEMENT_3D ( 'NONE', #3756, #15444, #2463 ) ;
#10374 = LINE ( 'NONE', #8777, #13894 ) ;
#10375 = CARTESIAN_POINT ( 'NONE',  ( -56.21322099054476240, -24.10372711620991382, 21.65063509461102242 ) ) ;
#10376 = EDGE_CURVE ( 'NONE', #7723, #16742, #7745, .T. ) ;
#10377 = DIRECTION ( 'NONE',  ( -0.9826218788918641422, -0.1856185419698762606, 0.000000000000000000 ) ) ;
#10378 = DIRECTION ( 'NONE',  ( -0.9876526153536336894, -0.1566598588826349503, 0.000000000000000000 ) ) ;
#10379 = ORIENTED_EDGE ( 'NONE', *, *, #7689, .F. ) ;
#10380 = ORIENTED_EDGE ( 'NONE', *, *, #8729, .F. ) ;
#10381 = CARTESIAN_POINT ( 'NONE',  ( -8.476787456656362352, -79.29982833240116236, 12.99038105676660848 ) ) ;
#10382 = VERTEX_POINT ( 'NONE', #16673 ) ;
#10383 = ORIENTED_EDGE ( 'NONE', *, *, #9492, .F. ) ;
#10384 = CIRCLE ( 'NONE', #13399, 1.500000000000001332 ) ;
#10385 = LINE ( 'NONE', #3096, #11088 ) ;
#10386 = DIRECTION ( 'NONE',  ( 0.9723968097209870765, 0.2333333333333371951, -2.660152884942554774E-16 ) ) ;
#10387 = APPLICATION_CONTEXT ( 'automotive_design' ) ;
#10388 = ADVANCED_FACE ( 'NONE', ( #18013 ), #13697, .F. ) ;
#10389 = DIRECTION ( 'NONE',  ( 0.9723968097209878536, -0.2333333333333339199, 0.000000000000000000 ) ) ;
#10390 = ORIENTED_EDGE ( 'NONE', *, *, #13342, .F. ) ;
#10391 = DIRECTION ( 'NONE',  ( -0.9876526153536336894, -0.1566598588826349503, 0.000000000000000000 ) ) ;
#10392 = CARTESIAN_POINT ( 'NONE',  ( -172.7326993491721225, 43.83249341393818810, 9.951701414186830458E-16 ) ) ;
#10393 = CARTESIAN_POINT ( 'NONE',  ( -74.48479437458692587, -27.00193450553860330, 21.65063509461101887 ) ) ;
#10394 = ORIENTED_EDGE ( 'NONE', *, *, #12968, .F. ) ;
#10395 = CARTESIAN_POINT ( 'NONE',  ( -49.01017969633304006, -28.02370111024093191, -21.65063509461098334 ) ) ;
#10396 = EDGE_CURVE ( 'NONE', #18395, #14596, #17347, .T. ) ;
#10397 = DIRECTION ( 'NONE',  ( -0.1566598588826321747, 0.9876526153536343555, 0.000000000000000000 ) ) ;
#10398 = FACE_BOUND ( 'NONE', #9704, .T. ) ;
#10399 = ORIENTED_EDGE ( 'NONE', *, *, #7642, .T. ) ;
#10401 = VERTEX_POINT ( 'NONE', #6155 ) ;
#10400 = CARTESIAN_POINT ( 'NONE',  ( -14.93616446663280328, -22.61893597879013740, 8.660254037844413944 ) ) ;
#10402 = ORIENTED_EDGE ( 'NONE', *, *, #3899, .F. ) ;
#10403 = CARTESIAN_POINT ( 'NONE',  ( -75.96627329761737712, -27.23692429386253266, -12.99038105676658006 ) ) ;
#10404 = EDGE_LOOP ( 'NONE', ( #13279, #11170, #12439, #9512, #2197, #16996, #11305, #11147, #2216, #1037 ) ) ;
#10405 = VERTEX_POINT ( 'NONE', #6346 ) ;
#10406 = CARTESIAN_POINT ( 'NONE',  ( -71.02801022084922522, -26.45362499944937440, -12.99038105676658006 ) ) ;
#10407 = EDGE_CURVE ( 'NONE', #450, #9967, #4894, .T. ) ;
#10408 = ORIENTED_EDGE ( 'NONE', *, *, #16598, .F. ) ;
#10409 = DIRECTION ( 'NONE',  ( -0.9876526153536336894, -0.1566598588826349503, 0.000000000000000000 ) ) ;
#10410 = ORIENTED_EDGE ( 'NONE', *, *, #12264, .T. ) ;
#10411 = CARTESIAN_POINT ( 'NONE',  ( -76.89338248673432474, -2.351275769351085732, -7.311503873159917788 ) ) ;
#10412 = EDGE_CURVE ( 'NONE', #1601, #13816, #7945, .T. ) ;
#10413 = PRODUCT_DEFINITION_CONTEXT ( 'detailed design', #11355, 'design' ) ;
#10414 = EDGE_CURVE ( 'NONE', #4333, #6623, #14601, .T. ) ;
#10415 = DIRECTION ( 'NONE',  ( -0.1566598588826321192, 0.9876526153536342445, 7.798540720466730171E-17 ) ) ;
#10416 = EDGE_CURVE ( 'NONE', #6562, #12633, #10654, .T. ) ;
#10417 = CARTESIAN_POINT ( 'NONE',  ( -30.53425299135042081, -20.03057078526148871, 17.32050807568881723 ) ) ;
#10418 = CARTESIAN_POINT ( 'NONE',  ( 73.09088021254186174, 1.387778780781445676E-14, 19.99999999999997513 ) ) ;
#10419 = AXIS2_PLACEMENT_3D ( 'NONE', #4734, #6185, #10518 ) ;
#10420 = ORIENTED_EDGE ( 'NONE', *, *, #13715, .T. ) ;
#10421 = EDGE_CURVE ( 'NONE', #13736, #12390, #18593, .T. ) ;
#10422 = CARTESIAN_POINT ( 'NONE',  ( -77.18258565727083464, 4.450738551673830479, -130.3485206753969976 ) ) ;
#10423 = ORIENTED_EDGE ( 'NONE', *, *, #10984, .T. ) ;
#10424 = DIRECTION ( 'NONE',  ( -0.1566598588826321747, 0.9876526153536343555, 0.000000000000000000 ) ) ;
#10425 = FACE_OUTER_BOUND ( 'NONE', #4652, .T. ) ;
#10426 = ORIENTED_EDGE ( 'NONE', *, *, #13629, .F. ) ;
#10427 = LINE ( 'NONE', #3314, #10156 ) ;
#10428 = ORIENTED_EDGE ( 'NONE', *, *, #16212, .T. ) ;
#10429 = ORIENTED_EDGE ( 'NONE', *, *, #13123, .T. ) ;
#10430 = EDGE_LOOP ( 'NONE', ( #2205, #7805 ) ) ;
#10431 = DIRECTION ( 'NONE',  ( 1.000000000000000000, 0.000000000000000000, 0.000000000000000000 ) ) ;
#10432 = ORIENTED_EDGE ( 'NONE', *, *, #16368, .T. ) ;
#10433 = AXIS2_PLACEMENT_3D ( 'NONE', #13128, #74, #4329 ) ;
#10434 = FACE_BOUND ( 'NONE', #12565, .T. ) ;
#10435 = DIRECTION ( 'NONE',  ( -0.1566598588826321747, 0.9876526153536343555, 0.000000000000000000 ) ) ;
#10436 = LINE ( 'NONE', #12217, #15203 ) ;
#10437 = EDGE_LOOP ( 'NONE', ( #13222, #2002, #5965, #17410 ) ) ;
#10438 = EDGE_CURVE ( 'NONE', #14662, #93, #11888, .T. ) ;
#10439 = VERTEX_POINT ( 'NONE', #12269 ) ;
#10440 = LINE ( 'NONE', #17875, #2475 ) ;
#10441 = EDGE_LOOP ( 'NONE', ( #910, #7383, #5979, #13352 ) ) ;
#10442 = DIRECTION ( 'NONE',  ( -2.887450008416415878E-16, -0.000000000000000000, -1.000000000000000000 ) ) ;
#10443 = AXIS2_PLACEMENT_3D ( 'NONE', #3334, #1927, #12036 ) ;
#10444 = CARTESIAN_POINT ( 'NONE',  ( 55.85952145814821534, 6.938893903907228378E-15, -2.500000000000000000 ) ) ;
#10445 = EDGE_CURVE ( 'NONE', #11399, #11897, #9350, .T. ) ;
#10446 = DIRECTION ( 'NONE',  ( 0.1856185419698760941, -0.9826218788918640312, 0.000000000000000000 ) ) ;
#10447 = DIRECTION ( 'NONE',  ( 0.000000000000000000, 0.000000000000000000, 1.000000000000000000 ) ) ;
#10448 = ADVANCED_BREP_SHAPE_REPRESENTATION ( '', ( #8769, #18772 ), #18155 ) ;
#10449 = CARTESIAN_POINT ( 'NONE',  ( -69.25705831108246002, -31.23522821733487476, 17.32050807568881723 ) ) ;
#10450 = VERTEX_POINT ( 'NONE', #15137 ) ;
#10451 = ORIENTED_EDGE ( 'NONE', *, *, #12615, .T. ) ;
#10452 = DIRECTION ( 'NONE',  ( -1.000000000000000000, -0.000000000000000000, -0.000000000000000000 ) ) ;
#10453 = CARTESIAN_POINT ( 'NONE',  ( -62.79768130110601021, -87.91612057094592103, 21.65063509461101532 ) ) ;
#10454 = DIRECTION ( 'NONE',  ( -0.1566598588826321192, 0.9876526153536342445, 7.798540720466730171E-17 ) ) ;
#10455 = CARTESIAN_POINT ( 'NONE',  ( -33.99103714508810725, -20.57888029135069630, 8.660254037844417496 ) ) ;
#10456 = EDGE_LOOP ( 'NONE', ( #4157, #14804 ) ) ;
#10457 = ORIENTED_EDGE ( 'NONE', *, *, #13737, .F. ) ;
#10458 = CARTESIAN_POINT ( 'NONE',  ( -44.56574292724170760, -27.31873174526908699, 1.869203119972154228E-14 ) ) ;
#10459 = CYLINDRICAL_SURFACE ( 'NONE', #16074, 1.500000000000001554 ) ;
#10460 = CARTESIAN_POINT ( 'NONE',  ( -81.73462711737164454, 33.01666666666666572, -35.00000000000000000 ) ) ;
#10461 = EDGE_LOOP ( 'NONE', ( #9269, #16426 ) ) ;
#10462 = AXIS2_PLACEMENT_3D ( 'NONE', #407, #17768, #4839 ) ;
#10463 = CARTESIAN_POINT ( 'NONE',  ( 0.5768043922889515285, -15.09578523045857601, 1.387778780781445676E-14 ) ) ;
#10464 = DIRECTION ( 'NONE',  ( 1.000000000000000000, 0.000000000000000000, 0.000000000000000000 ) ) ;
#10465 = EDGE_CURVE ( 'NONE', #6411, #16662, #12464, .T. ) ;
#10466 = DIRECTION ( 'NONE',  ( -0.1566598588826321747, 0.9876526153536343555, 0.000000000000000000 ) ) ;
#10467 = VERTEX_POINT ( 'NONE', #13416 ) ;
#10468 = EDGE_LOOP ( 'NONE', ( #7086, #11807, #2971, #13157 ) ) ;
#10469 = DIRECTION ( 'NONE',  ( -0.1566598588826321192, 0.9876526153536342445, 7.798540720466730171E-17 ) ) ;
#10470 = VERTEX_POINT ( 'NONE', #6241 ) ;
#10471 = AXIS2_PLACEMENT_3D ( 'NONE', #16676, #8128, #2621 ) ;
#10472 = ORIENTED_EDGE ( 'NONE', *, *, #10087, .T. ) ;
#10473 = EDGE_CURVE ( 'NONE', #7569, #2144, #4593, .T. ) ;
#10474 = ORIENTED_EDGE ( 'NONE', *, *, #12239, .F. ) ;
#10475 = CIRCLE ( 'NONE', #2310, 1.500000000000001332 ) ;
#10476 = DIRECTION ( 'NONE',  ( -0.1566598588826321747, 0.9876526153536343555, 0.000000000000000000 ) ) ;
#10477 = FACE_OUTER_BOUND ( 'NONE', #2781, .T. ) ;
#10478 = DIRECTION ( 'NONE',  ( 1.000000000000000000, 0.000000000000000000, 0.000000000000000000 ) ) ;
#10479 = AXIS2_PLACEMENT_3D ( 'NONE', #3355, #9620, #15115 ) ;
#10480 = PLANE ( 'NONE',  #16127 ) ;
#10481 = DIRECTION ( 'NONE',  ( -0.000000000000000000, -0.000000000000000000, 1.000000000000000000 ) ) ;
#10482 = CARTESIAN_POINT ( 'NONE',  ( -13.25033222266188560, -17.28902325481542235, 21.65063509461101177 ) ) ;
#10483 = FACE_OUTER_BOUND ( 'NONE', #122, .T. ) ;
#10484 = DIRECTION ( 'NONE',  ( 0.000000000000000000, 0.000000000000000000, -1.000000000000000000 ) ) ;
#10485 = CIRCLE ( 'NONE', #16249, 1.500000000000000000 ) ;
#10486 = FACE_BOUND ( 'NONE', #15764, .T. ) ;
#10487 = CIRCLE ( 'NONE', #2324, 2.000000000000000000 ) ;
#10488 = FACE_OUTER_BOUND ( 'NONE', #12125, .T. ) ;
#10489 = ORIENTED_EDGE ( 'NONE', *, *, #5792, .T. ) ;
#10490 = CIRCLE ( 'NONE', #12255, 1.500000000000001332 ) ;
#10492 = ORIENTED_EDGE ( 'NONE', *, *, #15162, .F. ) ;
#10491 = FACE_OUTER_BOUND ( 'NONE', #17979, .T. ) ;
#10493 = VERTEX_POINT ( 'NONE', #16385 ) ;
#10494 = DIRECTION ( 'NONE',  ( -0.9876526153536341335, -0.1566598588826327021, 0.000000000000000000 ) ) ;
#10495 = ORIENTED_EDGE ( 'NONE', *, *, #5714, .T. ) ;
#10496 = EDGE_CURVE ( 'NONE', #14458, #5860, #11256, .T. ) ;
#10497 = CIRCLE ( 'NONE', #9604, 1.500000000000000444 ) ;
#10498 = ORIENTED_EDGE ( 'NONE', *, *, #5615, .F. ) ;
#10499 = VECTOR ( 'NONE', #1481, 1000.000000000000114 ) ;
#10500 = VERTEX_POINT ( 'NONE', #1961 ) ;
#10501 = DIRECTION ( 'NONE',  ( -0.9876526153536336894, -0.1566598588826349503, 0.000000000000000000 ) ) ;
#10502 = ORIENTED_EDGE ( 'NONE', *, *, #18443, .F. ) ;
#10503 = CARTESIAN_POINT ( 'NONE',  ( -9.504075082187826595, -21.75730675493566579, -4.330127018922181215 ) ) ;
#10504 = ADVANCED_FACE ( 'NONE', ( #9644 ), #6617, .F. ) ;
#10505 = ORIENTED_EDGE ( 'NONE', *, *, #123, .F. ) ;
#10506 = TOROIDAL_SURFACE ( 'NONE', #9612, 3.000000000000000000, 2.000000000000000000 ) ;
#10507 = ORIENTED_EDGE ( 'NONE', *, *, #4474, .T. ) ;
#10508 = DIRECTION ( 'NONE',  ( -0.1566598588826321747, 0.9876526153536343555, 0.000000000000000000 ) ) ;
#10509 = DIRECTION ( 'NONE',  ( 0.000000000000000000, 0.000000000000000000, 1.000000000000000000 ) ) ;
#10510 = CARTESIAN_POINT ( 'NONE',  ( -129.1404785418517918, -14.43865647753341896, -5.316095106350545940 ) ) ;
#10511 = DIRECTION ( 'NONE',  ( -0.000000000000000000, -0.000000000000000000, -1.000000000000000000 ) ) ;
#10512 = CARTESIAN_POINT ( 'NONE',  ( -34.15575545585074480, -83.37298466334958391, -8.660254037844385522 ) ) ;
#10513 = DIRECTION ( 'NONE',  ( -0.9868632313631133801, -0.1615579233078773269, 0.000000000000000000 ) ) ;
#10514 = ORIENTED_EDGE ( 'NONE', *, *, #18077, .F. ) ;
#10515 = CIRCLE ( 'NONE', #5981, 1.499999999999999556 ) ;
#10516 = DIRECTION ( 'NONE',  ( -0.000000000000000000, -0.000000000000000000, -1.000000000000000000 ) ) ;
#10517 = VERTEX_POINT ( 'NONE', #1047 ) ;
#10518 = DIRECTION ( 'NONE',  ( 0.000000000000000000, 0.000000000000000000, 1.000000000000000000 ) ) ;
#10519 = DIRECTION ( 'NONE',  ( 0.000000000000000000, 0.000000000000000000, -1.000000000000000000 ) ) ;
#10520 = CIRCLE ( 'NONE', #9633, 2.000000000000000000 ) ;
#10521 = VERTEX_POINT ( 'NONE', #3831 ) ;
#10522 = DIRECTION ( 'NONE',  ( -0.1566598588826321192, 0.9876526153536342445, 7.798540720466730171E-17 ) ) ;
#10523 = ORIENTED_EDGE ( 'NONE', *, *, #16346, .T. ) ;
#10524 = ORIENTED_EDGE ( 'NONE', *, *, #11852, .F. ) ;
#10525 = FACE_OUTER_BOUND ( 'NONE', #10468, .T. ) ;
#10526 = EDGE_CURVE ( 'NONE', #9141, #4403, #13784, .T. ) ;
#10527 = ADVANCED_FACE ( 'NONE', ( #2443 ), #5192, .F. ) ;
#10528 = VERTEX_POINT ( 'NONE', #16778 ) ;
#10529 = FACE_BOUND ( 'NONE', #14322, .T. ) ;
#10530 = AXIS2_PLACEMENT_3D ( 'NONE', #7391, #16000, #4144 ) ;
#10531 = EDGE_CURVE ( 'NONE', #7400, #10171, #8553, .T. ) ;
#10532 = ORIENTED_EDGE ( 'NONE', *, *, #1411, .F. ) ;
#10533 = VERTEX_POINT ( 'NONE', #18606 ) ;
#10534 = VECTOR ( 'NONE', #8075, 1000.000000000000000 ) ;
#10535 = FACE_OUTER_BOUND ( 'NONE', #16206, .T. ) ;
#10536 = CARTESIAN_POINT ( 'NONE',  ( 0.4120860815263194254, -77.88988960245745830, -8.660254037844385522 ) ) ;
#10537 = DIRECTION ( 'NONE',  ( 1.000000000000000000, 0.000000000000000000, 0.000000000000000000 ) ) ;
#10538 = VECTOR ( 'NONE', #223, 1000.000000000000000 ) ;
#10539 = CARTESIAN_POINT ( 'NONE',  ( -56.21322099054479082, -24.10372711620990316, -4.330127018922180326 ) ) ;
#10540 = MECHANICAL_DESIGN_GEOMETRIC_PRESENTATION_REPRESENTATION (  '', ( #5726 ), #4484 ) ;
#10541 = B_SPLINE_CURVE_WITH_KNOTS ( 'NONE', 3,
 ( #10052, #9954, #8728, #15841, #1629, #15749, #2770, #8556, #7232, #14513, #1539, #13084, #11726, #10411, #4724, #3295 ),
 .UNSPECIFIED., .F., .F.,
 ( 4, 2, 2, 2, 2, 2, 2, 4 ),
 ( 0.000000000000000000, 0.001565668136846128924, 0.002348502205269182869, 0.003131336273692236598, 0.004697004410538344922, 0.005479838478961394747, 0.005871255513172918793, 0.006262672547384443705 ),
 .UNSPECIFIED. ) ;
#10542 = CARTESIAN_POINT ( 'NONE',  ( -63.78533391645962780, -88.07278042982852639, -17.32050807568878525 ) ) ;
#10543 = CARTESIAN_POINT ( 'NONE',  ( -88.14047854185180597, 6.938893903907228378E-15, 30.00000000000000000 ) ) ;
#10544 = VERTEX_POINT ( 'NONE', #2530 ) ;
#10545 = EDGE_LOOP ( 'NONE', ( #5038, #15871 ) ) ;
#10546 = DIRECTION ( 'NONE',  ( -0.1566598588826321192, 0.9876526153536342445, 7.798540720466730171E-17 ) ) ;
#10547 = CARTESIAN_POINT ( 'NONE',  ( -62.79768130110601021, -87.91612057094590682, 4.330127018922213189 ) ) ;
#10548 = FACE_OUTER_BOUND ( 'NONE', #3846, .T. ) ;
#10549 = CLOSED_SHELL ( 'NONE', ( #6225, #12001, #3061, #12616, #7543, #11856, #2487, #16720, #17958, #6493, #4038, #11913, #11206 ) ) ;
#10550 = ADVANCED_FACE ( 'NONE', ( #15318 ), #12478, .F. ) ;
#10551 = AXIS2_PLACEMENT_3D ( 'NONE', #18171, #899, #10909 ) ;
#10552 = VERTEX_POINT ( 'NONE', #18507 ) ;
#10553 = DIRECTION ( 'NONE',  ( -0.1566598588826321192, 0.9876526153536342445, 7.798540720466730171E-17 ) ) ;
#10554 = AXIS2_PLACEMENT_3D ( 'NONE', #262, #17444, #8710 ) ;
#10555 = VECTOR ( 'NONE', #3401, 1000.000000000000000 ) ;
#10556 = EDGE_CURVE ( 'NONE', #827, #8225, #3671, .T. ) ;
#10557 = CARTESIAN_POINT ( 'NONE',  ( -24.31886431249228409, -24.10720463817513703, 12.99038105676661736 ) ) ;
#10558 = DIRECTION ( 'NONE',  ( -0.1566598588826321192, 0.9876526153536342445, 7.798540720466730171E-17 ) ) ;
#10559 = CARTESIAN_POINT ( 'NONE',  ( -54.89646037827694869, -86.66284169988485075, 21.65063509461101532 ) ) ;
#10560 = CIRCLE ( 'NONE', #12979, 1.500000000000000000 ) ;
#10561 = DIRECTION ( 'NONE',  ( -0.9876526153536336894, -0.1566598588826349503, 0.000000000000000000 ) ) ;
#10563 = DIRECTION ( 'NONE',  ( -0.1566598588826321192, 0.9876526153536342445, 7.798540720466730171E-17 ) ) ;
#10562 = VECTOR ( 'NONE', #6558, 1000.000000000000000 ) ;
#10564 = DIRECTION ( 'NONE',  ( -0.1566598588826321192, 0.9876526153536342445, 7.798540720466730171E-17 ) ) ;
#10565 = AXIS2_PLACEMENT_3D ( 'NONE', #2336, #1048, #17058 ) ;
#10566 = VERTEX_POINT ( 'NONE', #2243 ) ;
#10567 = ORIENTED_EDGE ( 'NONE', *, *, #18157, .T. ) ;
#10568 = CYLINDRICAL_SURFACE ( 'NONE', #9099, 1.500000000000000666 ) ;
#10569 = AXIS2_PLACEMENT_3D ( 'NONE', #6131, #9048, #11871 ) ;
#10570 = CIRCLE ( 'NONE', #2402, 1.500000000000001332 ) ;
#10571 = ORIENTED_EDGE ( 'NONE', *, *, #12541, .F. ) ;
#10572 = ORIENTED_EDGE ( 'NONE', *, *, #15672, .F. ) ;
#10573 = ORIENTED_EDGE ( 'NONE', *, *, #16548, .T. ) ;
#10574 = AXIS2_PLACEMENT_3D ( 'NONE', #14351, #4300, #10072 ) ;
#10575 = CIRCLE ( 'NONE', #2413, 1.500000000000000888 ) ;
#10576 = CARTESIAN_POINT ( 'NONE',  ( -30.69897130211303349, -82.82467515726038698, 17.32050807568881368 ) ) ;
#10577 = EDGE_CURVE ( 'NONE', #2139, #272, #16725, .T. ) ;
#10578 = ORIENTED_EDGE ( 'NONE', *, *, #1871, .T. ) ;
#10579 = CIRCLE ( 'NONE', #3306, 1.500000000000001332 ) ;
#10580 = EDGE_CURVE ( 'NONE', #3795, #6562, #5477, .T. ) ;
#10581 = PLANE ( 'NONE',  #14333 ) ;
#10582 = CIRCLE ( 'NONE', #1531, 1.500000000000001332 ) ;
#10583 = DIRECTION ( 'NONE',  ( -0.9876526153536336894, -0.1566598588826349503, 0.000000000000000000 ) ) ;
#10584 = ORIENTED_EDGE ( 'NONE', *, *, #1580, .T. ) ;
#10585 = SHAPE_REPRESENTATION ( 'Heavy Presser Piston Block', ( #18772 ), #17189 ) ;
#10586 = PRODUCT_DEFINITION_SHAPE ( 'NONE', 'NONE',  #16949 ) ;
#10587 = ADVANCED_FACE ( 'NONE', ( #15594 ), #6907, .F. ) ;
#10588 = DIRECTION ( 'NONE',  ( -0.1566598588826321192, 0.9876526153536342445, 7.798540720466730171E-17 ) ) ;
#10589 = ORIENTED_EDGE ( 'NONE', *, *, #2462, .F. ) ;
#10590 = LINE ( 'NONE', #9259, #17764 ) ;
#10591 = AXIS2_PLACEMENT_3D ( 'NONE', #18010, #3827, #5376 ) ;
#10592 = DIRECTION ( 'NONE',  ( -0.9876526153536336894, -0.1566598588826350336, 0.000000000000000000 ) ) ;
#10593 = CARTESIAN_POINT ( 'NONE',  ( -19.87442754340095519, -23.40223527320329922, 17.32050807568881012 ) ) ;
#10594 = VECTOR ( 'NONE', #462, 1000.000000000000000 ) ;
#10595 = CYLINDRICAL_SURFACE ( 'NONE', #15646, 1.500000000000001554 ) ;
#10597 = ORIENTED_EDGE ( 'NONE', *, *, #7448, .F. ) ;
#10596 = DIRECTION ( 'NONE',  ( -0.1566598588826321192, 0.9876526153536342445, 7.798540720466731404E-17 ) ) ;
#10598 = VERTEX_POINT ( 'NONE', #11036 ) ;
#10599 = AXIS2_PLACEMENT_3D ( 'NONE', #13106, #7082, #13011 ) ;
#10600 = FACE_OUTER_BOUND ( 'NONE', #12489, .T. ) ;
#10601 = ORIENTED_EDGE ( 'NONE', *, *, #11151, .F. ) ;
#10602 = ORIENTED_EDGE ( 'NONE', *, *, #9152, .F. ) ;
#10603 = VERTEX_POINT ( 'NONE', #11237 ) ;
#10604 = ORIENTED_EDGE ( 'NONE', *, *, #463, .T. ) ;
#10605 = DIRECTION ( 'NONE',  ( -0.9826218788918642533, -0.1856185419698762884, 0.000000000000000000 ) ) ;
#10606 = DIRECTION ( 'NONE',  ( -0.1566598588826321192, 0.9876526153536342445, 7.798540720466730171E-17 ) ) ;
#10607 = ORIENTED_EDGE ( 'NONE', *, *, #15478, .F. ) ;
#10608 = CARTESIAN_POINT ( 'NONE',  ( -15.92381708198642798, -22.77559583767277473, -21.65063509461098334 ) ) ;
#10609 = AXIS2_PLACEMENT_3D ( 'NONE', #15324, #950, #2339 ) ;
#10610 = DIRECTION ( 'NONE',  ( -0.9876526153536341335, -0.1566598588826327021, 0.000000000000000000 ) ) ;
#10611 = CARTESIAN_POINT ( 'NONE',  ( -70.00000000000000000, 44.99999999999999289, 25.00000000000000000 ) ) ;
#10612 = EDGE_CURVE ( 'NONE', #1825, #11443, #4302, .T. ) ;
#10613 = DIRECTION ( 'NONE',  ( -0.1566598588826321747, 0.9876526153536343555, 0.000000000000000000 ) ) ;
#10614 = FACE_OUTER_BOUND ( 'NONE', #4882, .T. ) ;
#10615 = ORIENTED_EDGE ( 'NONE', *, *, #13745, .F. ) ;
#10616 = VECTOR ( 'NONE', #16769, 1000.000000000000000 ) ;
#10617 = CARTESIAN_POINT ( 'NONE',  ( -56.21322099054479082, -24.10372711620989605, -21.65063509461097979 ) ) ;
#10618 = ORIENTED_EDGE ( 'NONE', *, *, #9005, .T. ) ;
#10619 = CYLINDRICAL_SURFACE ( 'NONE', #8329, 1.500000000000000666 ) ;
#10620 = ADVANCED_FACE ( 'NONE', ( #16864 ), #15515, .F. ) ;
#10621 = AXIS2_PLACEMENT_3D ( 'NONE', #4613, #7387, #17817 ) ;
#10622 = CARTESIAN_POINT ( 'NONE',  ( -129.1404785418517918, -14.35070196317933267, -5.500000000000000000 ) ) ;
#10623 = ORIENTED_EDGE ( 'NONE', *, *, #15045, .T. ) ;
#10624 = ORIENTED_EDGE ( 'NONE', *, *, #9156, .F. ) ;
#10625 = ORIENTED_EDGE ( 'NONE', *, *, #690, .F. ) ;
#10626 = VERTEX_POINT ( 'NONE', #14083 ) ;
#10627 = DIRECTION ( 'NONE',  ( -0.9876526153536341335, -0.1566598588826327021, 0.000000000000000000 ) ) ;
#10628 = AXIS2_PLACEMENT_3D ( 'NONE', #4115, #5571, #17138 ) ;
#10629 = VERTEX_POINT ( 'NONE', #5379 ) ;
#10630 = FACE_BOUND ( 'NONE', #7213, .T. ) ;
#10631 = CIRCLE ( 'NONE', #17324, 1.500000000000000888 ) ;
#10632 = ORIENTED_EDGE ( 'NONE', *, *, #13766, .T. ) ;
#10633 = SURFACE_STYLE_FILL_AREA ( #16232 ) ;
#10634 = EDGE_CURVE ( 'NONE', #6863, #17521, #4025, .T. ) ;
#10635 = VERTEX_POINT ( 'NONE', #1130 ) ;
#10636 = CIRCLE ( 'NONE', #3967, 1.500000000000000888 ) ;
#10637 = CIRCLE ( 'NONE', #16405, 1.500000000000000444 ) ;
#10638 = EDGE_CURVE ( 'NONE', #6457, #17941, #9766, .T. ) ;
#10639 = ORIENTED_EDGE ( 'NONE', *, *, #5490, .T. ) ;
#10640 = EDGE_CURVE ( 'NONE', #6894, #8134, #16424, .T. ) ;
#10641 = DIRECTION ( 'NONE',  ( -0.9876526153536341335, -0.1566598588826327021, 0.000000000000000000 ) ) ;
#10642 = CARTESIAN_POINT ( 'NONE',  ( -15.92381708198643153, -22.77559583767277473, 12.99038105676661381 ) ) ;
#10643 = EDGE_CURVE ( 'NONE', #5513, #2328, #12154, .T. ) ;
#10644 = CIRCLE ( 'NONE', #15799, 1.500000000000000888 ) ;
#10645 = CARTESIAN_POINT ( 'NONE',  ( -74.01655979591544110, 46.70906433774060673, -2.532234642382003909 ) ) ;
#10646 = CARTESIAN_POINT ( 'NONE',  ( -65.30644784966793281, -30.60858878180435738, -12.99038105676658006 ) ) ;
#10647 = ORIENTED_EDGE ( 'NONE', *, *, #6884, .T. ) ;
#10648 = ORIENTED_EDGE ( 'NONE', *, *, #7635, .F. ) ;
#10649 = FACE_OUTER_BOUND ( 'NONE', #8965, .T. ) ;
#10650 = CARTESIAN_POINT ( 'NONE',  ( -65.10209452872744862, -25.51366584615359656, 17.32050807568881723 ) ) ;
#10651 = AXIS2_PLACEMENT_3D ( 'NONE', #12298, #9572, #2361 ) ;
#10652 = ORIENTED_EDGE ( 'NONE', *, *, #10884, .T. ) ;
#10653 = CARTESIAN_POINT ( 'NONE',  ( -51.97313754239392836, -28.49368068688882971, -4.330127018922181215 ) ) ;
#10654 = CIRCLE ( 'NONE', #1878, 1.500000000000000000 ) ;
#10655 = DIRECTION ( 'NONE',  ( -0.1566598588826321192, 0.9876526153536342445, 7.798540720466730171E-17 ) ) ;
#10656 = CARTESIAN_POINT ( 'NONE',  ( -90.00000000000000000, 34.99999999999999289, -35.00000000000000000 ) ) ;
#10657 = DIRECTION ( 'NONE',  ( -0.1566598588826321192, 0.9876526153536342445, 7.798540720466730171E-17 ) ) ;
#10658 = FILL_AREA_STYLE_COLOUR ( '', #6906 ) ;
#10659 = EDGE_CURVE ( 'NONE', #9088, #4142, #3250, .T. ) ;
#10660 = EDGE_CURVE ( 'NONE', #1682, #3315, #6962, .T. ) ;
#10661 = ADVANCED_FACE ( 'NONE', ( #17339 ), #2715, .T. ) ;
#10662 = CARTESIAN_POINT ( 'NONE',  ( -45.34904222165486942, -22.38046866850095284, -8.660254037844380193 ) ) ;
#10663 = CYLINDRICAL_SURFACE ( 'NONE', #5663, 1.500000000000001554 ) ;
#10664 = CARTESIAN_POINT ( 'NONE',  ( -29.25712738926042888, -24.89050393258829175, -12.99038105676658006 ) ) ;
#10665 = VERTEX_POINT ( 'NONE', #14463 ) ;
#10666 = AXIS2_PLACEMENT_3D ( 'NONE', #11366, #14332, #4276 ) ;
#10667 = CARTESIAN_POINT ( 'NONE',  ( -61.31620237807555895, -87.68113078262194904, -12.99038105676658539 ) ) ;
#10668 = ORIENTED_EDGE ( 'NONE', *, *, #1940, .T. ) ;
#10669 = EDGE_LOOP ( 'NONE', ( #6316, #612, #8721, #15311 ) ) ;
#10670 = VERTEX_POINT ( 'NONE', #4222 ) ;
#10671 = CARTESIAN_POINT ( 'NONE',  ( -69.99999999999998579, -45.00000000000000711, -19.99999999999999645 ) ) ;
#10672 = CARTESIAN_POINT ( 'NONE',  ( -30.53425299135042081, -20.03057078526148160, 1.908195823574487804E-14 ) ) ;
#10673 = VERTEX_POINT ( 'NONE', #13121 ) ;
#10674 = DIRECTION ( 'NONE',  ( 0.9868632313631133801, -0.1615579233078772714, 2.999697980758352134E-17 ) ) ;
#10675 = VECTOR ( 'NONE', #16489, 1000.000000000000000 ) ;
#10676 = DIRECTION ( 'NONE',  ( 0.000000000000000000, 0.000000000000000000, 1.000000000000000000 ) ) ;
#10677 = ORIENTED_EDGE ( 'NONE', *, *, #8184, .F. ) ;
#10678 = CARTESIAN_POINT ( 'NONE',  ( -70.20507591625822386, -89.09106951256565310, 17.32050807568881368 ) ) ;
#10679 = DIRECTION ( 'NONE',  ( 0.000000000000000000, 0.000000000000000000, 1.000000000000000000 ) ) ;
#10680 = DIRECTION ( 'NONE',  ( -0.1566598588826321192, 0.9876526153536342445, 7.798540720466730171E-17 ) ) ;
#10681 = CYLINDRICAL_SURFACE ( 'NONE', #6245, 1.500000000000001554 ) ;
#10682 = CARTESIAN_POINT ( 'NONE',  ( 0.4120860815263194254, -77.88988960245745830, 17.32050807568880657 ) ) ;
#10683 = CARTESIAN_POINT ( 'NONE',  ( -17.40529600501687923, -23.01058562599671831, -21.65063509461098334 ) ) ;
#10684 = DIRECTION ( 'NONE',  ( 0.000000000000000000, 0.000000000000000000, 1.000000000000000000 ) ) ;
#10686 = VERTEX_POINT ( 'NONE', #2979 ) ;
#10685 = CARTESIAN_POINT ( 'NONE',  ( 0.000000000000000000, 0.000000000000000000, -40.65685424949239035 ) ) ;
#10687 = ADVANCED_FACE ( 'NONE', ( #4116 ), #10097, .F. ) ;
#10688 = EDGE_CURVE ( 'NONE', #3161, #11647, #5852, .T. ) ;
#10689 = DIRECTION ( 'NONE',  ( 0.9201637183752249260, -0.3915338189555017667, 0.000000000000000000 ) ) ;
#10690 = VECTOR ( 'NONE', #2833, 1000.000000000000000 ) ;
#10691 = ORIENTED_EDGE ( 'NONE', *, *, #6465, .F. ) ;
#10692 = VERTEX_POINT ( 'NONE', #8510 ) ;
#10693 = VERTEX_POINT ( 'NONE', #8873 ) ;
#10694 = CARTESIAN_POINT ( 'NONE',  ( -84.23462711737164454, 33.01666666666666572, -30.00000000000000000 ) ) ;
#10695 = DIRECTION ( 'NONE',  ( -0.1566598588826321747, 0.9876526153536343555, 0.000000000000000000 ) ) ;
#10696 = DIRECTION ( 'NONE',  ( 1.000000000000000000, 0.000000000000000000, 0.000000000000000000 ) ) ;
#10697 = CARTESIAN_POINT ( 'NONE',  ( -346.6567719130321166, 10.97801148527007697, 9.951701414186830458E-16 ) ) ;
#10698 = DIRECTION ( 'NONE',  ( -0.9710487832595061652, 0.2388812686885108671, -1.247264370992099311E-16 ) ) ;
#10699 = DIRECTION ( 'NONE',  ( -0.9876526153536341335, -0.1566598588826327021, 0.000000000000000000 ) ) ;
#10700 = CARTESIAN_POINT ( 'NONE',  ( -48.02252708097939404, -27.86704125135830523, 17.32050807568881723 ) ) ;
#10701 = DIRECTION ( 'NONE',  ( 1.000000000000000000, 0.000000000000000000, -2.631994239413086031E-16 ) ) ;
#10702 = EDGE_CURVE ( 'NONE', #3364, #931, #12321, .T. ) ;
#10703 = CARTESIAN_POINT ( 'NONE',  ( -32.22008523532134205, -25.36048350923618955, 21.65063509461101887 ) ) ;
#10704 = EDGE_LOOP ( 'NONE', ( #10106, #11747 ) ) ;
#10705 = ORIENTED_EDGE ( 'NONE', *, *, #13651, .F. ) ;
#10706 = VERTEX_POINT ( 'NONE', #15803 ) ;
#10707 = DIRECTION ( 'NONE',  ( 1.000000000000000000, 0.000000000000000000, 0.000000000000000000 ) ) ;
#10708 = EDGE_CURVE ( 'NONE', #2965, #13292, #12988, .T. ) ;
#10709 = FACE_BOUND ( 'NONE', #17111, .T. ) ;
#10710 = FACE_OUTER_BOUND ( 'NONE', #12613, .T. ) ;
#10711 = EDGE_CURVE ( 'NONE', #2692, #3641, #13895, .T. ) ;
#10712 = VERTEX_POINT ( 'NONE', #4324 ) ;
#10713 = ORIENTED_EDGE ( 'NONE', *, *, #3850, .T. ) ;
#10714 = FACE_OUTER_BOUND ( 'NONE', #776, .T. ) ;
#10715 = DIRECTION ( 'NONE',  ( 0.000000000000000000, 0.000000000000000000, 1.000000000000000000 ) ) ;
#10716 = DIRECTION ( 'NONE',  ( -0.9826218788918642533, -0.1856185419698762884, 0.000000000000000000 ) ) ;
#10717 = FACE_OUTER_BOUND ( 'NONE', #11632, .T. ) ;
#10718 = DIRECTION ( 'NONE',  ( 0.000000000000000000, 0.000000000000000000, -1.000000000000000000 ) ) ;
#10719 = ORIENTED_EDGE ( 'NONE', *, *, #3610, .T. ) ;
#10720 = EDGE_LOOP ( 'NONE', ( #11689, #2009 ) ) ;
#10721 = DIRECTION ( 'NONE',  ( 0.000000000000000000, 0.000000000000000000, 1.000000000000000000 ) ) ;
#10722 = CIRCLE ( 'NONE', #6507, 1.500000000000000888 ) ;
#10723 = CARTESIAN_POINT ( 'NONE',  ( -66.29410046502155751, -30.76524864068697696, 1.887572821959364500E-14 ) ) ;
#10724 = ORIENTED_EDGE ( 'NONE', *, *, #14184, .T. ) ;
#10725 = ORIENTED_EDGE ( 'NONE', *, *, #2998, .F. ) ;
#10726 = ADVANCED_FACE ( 'NONE', ( #11678 ), #10282, .F. ) ;
#10727 = ORIENTED_EDGE ( 'NONE', *, *, #5588, .F. ) ;
#10728 = PLANE ( 'NONE',  #12437 ) ;
#10729 = FACE_OUTER_BOUND ( 'NONE', #4925, .T. ) ;
#10730 = EDGE_CURVE ( 'NONE', #1541, #2560, #6609, .T. ) ;
#10731 = AXIS2_PLACEMENT_3D ( 'NONE', #5775, #16177, #10101 ) ;
#10732 = CARTESIAN_POINT ( 'NONE',  ( -38.14600092744309734, -26.30044266253198160, 1.175313729581431390E-14 ) ) ;
#10733 = ORIENTED_EDGE ( 'NONE', *, *, #9925, .F. ) ;
#10734 = CARTESIAN_POINT ( 'NONE',  ( -58.68235252892886678, -24.49537676341648051, -8.660254037844380193 ) ) ;
#10735 = CARTESIAN_POINT ( 'NONE',  ( -39.62747985047357702, -26.53543245085592517, -17.32050807568878170 ) ) ;
#10736 = DIRECTION ( 'NONE',  ( -0.1566598588826321192, 0.9876526153536342445, 7.798540720466730171E-17 ) ) ;
#10737 = DIRECTION ( 'NONE',  ( -0.9876526153536336894, -0.1566598588826349503, 0.000000000000000000 ) ) ;
#10738 = EDGE_LOOP ( 'NONE', ( #12547, #15089 ) ) ;
#10739 = EDGE_LOOP ( 'NONE', ( #16957, #1403, #16667, #15563 ) ) ;
#10740 = LINE ( 'NONE', #352, #15761 ) ;
#10741 = ORIENTED_EDGE ( 'NONE', *, *, #18523, .F. ) ;
#10742 = CARTESIAN_POINT ( 'NONE',  ( 5.350349158294472218, -77.10659030804430358, 17.32050807568880657 ) ) ;
#10743 = VECTOR ( 'NONE', #3235, 1000.000000000000000 ) ;
#10744 = ORIENTED_EDGE ( 'NONE', *, *, #10412, .T. ) ;
#10745 = EDGE_CURVE ( 'NONE', #12642, #5059, #14378, .T. ) ;
#10746 = EDGE_CURVE ( 'NONE', #16739, #405, #3291, .T. ) ;
#10747 = CARTESIAN_POINT ( 'NONE',  ( -66.08974714408108753, -25.67032570503621614, -12.99038105676658006 ) ) ;
#10748 = EDGE_CURVE ( 'NONE', #16279, #5230, #13281, .T. ) ;
#10749 = LINE ( 'NONE', #15416, #2430 ) ;
#10750 = CYLINDRICAL_SURFACE ( 'NONE', #4338, 3.000000000000001776 ) ;
#10751 = DIRECTION ( 'NONE',  ( 0.000000000000000000, 0.000000000000000000, 1.000000000000000000 ) ) ;
#10752 = DIRECTION ( 'NONE',  ( -0.1566598588826321192, 0.9876526153536342445, 7.798540720466730171E-17 ) ) ;
#10753 = CYLINDRICAL_SURFACE ( 'NONE', #6950, 1.500000000000001554 ) ;
#10754 = CIRCLE ( 'NONE', #15614, 1.500000000000000888 ) ;
#10755 = DIRECTION ( 'NONE',  ( -0.1566598588826321192, 0.9876526153536342445, 7.798540720466730171E-17 ) ) ;
#10756 = CYLINDRICAL_SURFACE ( 'NONE', #7229, 1.500000000000000888 ) ;
#10757 = DIRECTION ( 'NONE',  ( -0.9876526153536336894, -0.1566598588826349503, 0.000000000000000000 ) ) ;
#10759 = ORIENTED_EDGE ( 'NONE', *, *, #6058, .F. ) ;
#10758 = DIRECTION ( 'NONE',  ( -0.9876526153536341335, -0.1566598588826327576, 0.000000000000000000 ) ) ;
#10760 = CARTESIAN_POINT ( 'NONE',  ( -62.00000000000000000, 0.000000000000000000, -25.00000000000000000 ) ) ;
#10761 = VECTOR ( 'NONE', #6846, 1000.000000000000000 ) ;
#10762 = ORIENTED_EDGE ( 'NONE', *, *, #14228, .T. ) ;
#10764 = ORIENTED_EDGE ( 'NONE', *, *, #596, .T. ) ;
#10763 = ADVANCED_FACE ( 'NONE', ( #1588 ), #9908, .F. ) ;
#10765 = ADVANCED_FACE ( 'NONE', ( #12846 ), #11410, .F. ) ;
#10766 = ORIENTED_EDGE ( 'NONE', *, *, #555, .F. ) ;
#10767 = CARTESIAN_POINT ( 'NONE',  ( -12.46703292824873088, -22.22728633158356359, -21.65063509461098334 ) ) ;
#10768 = CARTESIAN_POINT ( 'NONE',  ( -33.99103714508810725, -20.57888029135069985, 17.32050807568882078 ) ) ;
#10769 = DIRECTION ( 'NONE',  ( -0.9876526153536344665, -0.1566598588826304539, 0.000000000000000000 ) ) ;
#10770 = FACE_OUTER_BOUND ( 'NONE', #3788, .T. ) ;
#10771 = EDGE_CURVE ( 'NONE', #17353, #2946, #16281, .T. ) ;
#10772 = CARTESIAN_POINT ( 'NONE',  ( -128.0167453206627783, -15.18310030011310729, -3.150553392547042808 ) ) ;
#10773 = AXIS2_PLACEMENT_3D ( 'NONE', #6260, #10605, #3197 ) ;
#10774 = CARTESIAN_POINT ( 'NONE',  ( -89.14047854185180597, 6.938893903907228378E-15, 30.00000000000002487 ) ) ;
#10775 = EDGE_LOOP ( 'NONE', ( #7139, #1937 ) ) ;
#10776 = DIRECTION ( 'NONE',  ( -0.1566598588826321747, 0.9876526153536343555, 0.000000000000000000 ) ) ;
#10777 = ORIENTED_EDGE ( 'NONE', *, *, #14901, .T. ) ;
#10778 = FACE_BOUND ( 'NONE', #12425, .T. ) ;
#10779 = FACE_OUTER_BOUND ( 'NONE', #3216, .T. ) ;
#10780 = CARTESIAN_POINT ( 'NONE',  ( -129.1404785418517918, 52.54032238931508658, -2.500000000000000000 ) ) ;
#10781 = DIRECTION ( 'NONE',  ( 0.000000000000000000, 0.000000000000000000, 1.000000000000000000 ) ) ;
#10782 = VECTOR ( 'NONE', #18195, 1000.000000000000000 ) ;
#10783 = AXIS2_PLACEMENT_3D ( 'NONE', #10760, #6452, #751 ) ;
#10784 = VERTEX_POINT ( 'NONE', #3349 ) ;
#10785 = CARTESIAN_POINT ( 'NONE',  ( -88.14047854185180597, -33.59999999999994458, 25.00000000000001776 ) ) ;
#10786 = ORIENTED_EDGE ( 'NONE', *, *, #11593, .T. ) ;
#10787 = ORIENTED_EDGE ( 'NONE', *, *, #7756, .F. ) ;
#10788 = ORIENTED_EDGE ( 'NONE', *, *, #631, .T. ) ;
#10789 = ORIENTED_EDGE ( 'NONE', *, *, #101, .T. ) ;
#10790 = ORIENTED_EDGE ( 'NONE', *, *, #6908, .T. ) ;
#10791 = DIRECTION ( 'NONE',  ( 0.000000000000000000, 0.000000000000000000, 1.000000000000000000 ) ) ;
#10792 = VECTOR ( 'NONE', #12965, 1000.000000000000000 ) ;
#10793 = FACE_BOUND ( 'NONE', #8608, .T. ) ;
#10794 = CARTESIAN_POINT ( 'NONE',  ( -66.25446545484369665, -88.46443007703511796, -4.330127018922185655 ) ) ;
#10795 =( NAMED_UNIT ( * ) PLANE_ANGLE_UNIT ( ) SI_UNIT ( $, .RADIAN. ) );
#10796 = PRESENTATION_LAYER_ASSIGNMENT (  '', '', ( #3830 ) ) ;
#10797 = ORIENTED_EDGE ( 'NONE', *, *, #14791, .F. ) ;
#10798 = EDGE_CURVE ( 'NONE', #3227, #10224, #8115, .T. ) ;
#10799 = CIRCLE ( 'NONE', #15656, 2.000000000000000000 ) ;
#10800 = FACE_BOUND ( 'NONE', #16487, .T. ) ;
#10801 = EDGE_CURVE ( 'NONE', #10229, #12874, #12665, .T. ) ;
#10802 = DIRECTION ( 'NONE',  ( 0.9868632313631133801, -0.1615579233078772714, 0.000000000000000000 ) ) ;
#10803 = LINE ( 'NONE', #7899, #14822 ) ;
#10804 = CARTESIAN_POINT ( 'NONE',  ( 3.267113004676621661E-15, 1.140077944303684267E-15, -20.00000000000000355 ) ) ;
#10805 = CARTESIAN_POINT ( 'NONE',  ( -17.85948730251583783, -80.78809699178616199, -8.660254037844385522 ) ) ;
#10806 = ORIENTED_EDGE ( 'NONE', *, *, #12886, .F. ) ;
#10807 = DIRECTION ( 'NONE',  ( -1.000000000000000000, 0.000000000000000000, 0.000000000000000000 ) ) ;
#10808 = AXIS2_PLACEMENT_3D ( 'NONE', #18688, #2814, #12929 ) ;
#10809 = LINE ( 'NONE', #4670, #13912 ) ;
#10810 = AXIS2_PLACEMENT_3D ( 'NONE', #3395, #3856, #10875 ) ;
#10811 = DIRECTION ( 'NONE',  ( 0.000000000000000000, 0.000000000000000000, 1.000000000000000000 ) ) ;
#10812 = ORIENTED_EDGE ( 'NONE', *, *, #16935, .F. ) ;
#10813 = DIRECTION ( 'NONE',  ( -0.9876526153536341335, -0.1566598588826327021, 0.000000000000000000 ) ) ;
#10814 = CARTESIAN_POINT ( 'NONE',  ( -73.49714175923330117, -26.84527464665595531, -8.660254037844380193 ) ) ;
#10815 = CARTESIAN_POINT ( 'NONE',  ( -172.4933171327469097, 56.54760101112823634, -2.520603730400377884 ) ) ;
#10816 = VERTEX_POINT ( 'NONE', #16536 ) ;
#10817 = FACE_BOUND ( 'NONE', #13393, .T. ) ;
#10818 = CIRCLE ( 'NONE', #9024, 1.499999999999999556 ) ;
#10819 = DIRECTION ( 'NONE',  ( -0.000000000000000000, -0.000000000000000000, -1.000000000000000000 ) ) ;
#10820 = AXIS2_PLACEMENT_3D ( 'NONE', #1806, #17318, #9885 ) ;
#10821 = CARTESIAN_POINT ( 'NONE',  ( -56.41757431148526081, -29.19865005186066753, -17.32050807568878170 ) ) ;
#10822 = LINE ( 'NONE', #11108, #18183 ) ;
#10823 = CARTESIAN_POINT ( 'NONE',  ( 0.000000000000000000, 0.000000000000000000, 0.000000000000000000 ) ) ;
#10824 = AXIS2_PLACEMENT_3D ( 'NONE', #3101, #7035, #6443 ) ;
#10825 = ORIENTED_EDGE ( 'NONE', *, *, #2005, .F. ) ;
#10826 = EDGE_CURVE ( 'NONE', #14760, #10382, #9155, .T. ) ;
#10827 = DIRECTION ( 'NONE',  ( -0.1566598588826321192, 0.9876526153536342445, 7.798540720466731404E-17 ) ) ;
#10828 = CARTESIAN_POINT ( 'NONE',  ( 1.399738696879940791, -77.73322974357483872, 12.99038105676660493 ) ) ;
#10829 = CARTESIAN_POINT ( 'NONE',  ( -129.1404785418517918, -2.850701963179328668, 9.951701414186818625E-16 ) ) ;
#10830 = CIRCLE ( 'NONE', #13573, 1.500000000000000888 ) ;
#10831 = CARTESIAN_POINT ( 'NONE',  ( -61.15148406731292852, -24.88702641062307208, 21.65063509461102242 ) ) ;
#10832 = ORIENTED_EDGE ( 'NONE', *, *, #10953, .F. ) ;
#10833 = ORIENTED_EDGE ( 'NONE', *, *, #8069, .T. ) ;
#10834 = DIRECTION ( 'NONE',  ( -0.1566598588826321747, 0.9876526153536343555, 0.000000000000000000 ) ) ;
#10835 = CARTESIAN_POINT ( 'NONE',  ( -72.50948914387967648, -26.68861478777333218, 12.99038105676661736 ) ) ;
#10836 = VECTOR ( 'NONE', #1816, 1000.000000000000000 ) ;
#10837 = VERTEX_POINT ( 'NONE', #7822 ) ;
#10838 = EDGE_CURVE ( 'NONE', #11621, #15511, #11463, .T. ) ;
#10839 = CIRCLE ( 'NONE', #17237, 1.499999999999999556 ) ;
#10840 = EDGE_LOOP ( 'NONE', ( #11024, #8635, #15186, #5293 ) ) ;
#10841 = CARTESIAN_POINT ( 'NONE',  ( -71.23236354178969520, -31.54854793510013877, -17.32050807568878170 ) ) ;
#10842 = AXIS2_PLACEMENT_3D ( 'NONE', #17482, #4473, #13182 ) ;
#10843 = DIRECTION ( 'NONE',  ( 0.000000000000000000, 0.000000000000000000, 1.000000000000000000 ) ) ;
#10844 = CARTESIAN_POINT ( 'NONE',  ( 8.807133312032172867, -76.55828080195509244, 9.043241838514131834E-15 ) ) ;
#10845 = CARTESIAN_POINT ( 'NONE',  ( -39.13365354279672914, -26.45710252141460828, 12.99038105676661736 ) ) ;
#10846 = CIRCLE ( 'NONE', #12981, 1.500000000000000888 ) ;
#10847 = ORIENTED_EDGE ( 'NONE', *, *, #3852, .F. ) ;
#10848 = CARTESIAN_POINT ( 'NONE',  ( -1.892327146095121204, -15.48743487766515337, -12.99038105676658361 ) ) ;
#10849 = AXIS2_PLACEMENT_3D ( 'NONE', #18221, #5195, #16866 ) ;
#10850 = CIRCLE ( 'NONE', #11426, 1.500000000000000000 ) ;
#10851 = CARTESIAN_POINT ( 'NONE',  ( -309.1404785418517918, -2.850701963179328668, 9.951701414186818625E-16 ) ) ;
#10852 = AXIS2_PLACEMENT_3D ( 'NONE', #13397, #3526, #12243 ) ;
#10853 = CYLINDRICAL_SURFACE ( 'NONE', #10471, 1.500000000000001554 ) ;
#10854 = FACE_BOUND ( 'NONE', #12701, .T. ) ;
#10855 = EDGE_CURVE ( 'NONE', #6097, #9271, #17903, .T. ) ;
#10856 = DIRECTION ( 'NONE',  ( -0.000000000000000000, -0.000000000000000000, -1.000000000000000000 ) ) ;
#10857 = CARTESIAN_POINT ( 'NONE',  ( -36.66452200441264608, -26.06545287420802737, 1.193683431568641663E-14 ) ) ;
#10858 = EDGE_CURVE ( 'NONE', #3849, #15836, #7645, .T. ) ;
#10859 = ORIENTED_EDGE ( 'NONE', *, *, #17660, .T. ) ;
#10860 = EDGE_CURVE ( 'NONE', #16572, #8813, #4166, .T. ) ;
#10861 = CIRCLE ( 'NONE', #12675, 15.88900348692940945 ) ;
#10862 = VERTEX_POINT ( 'NONE', #13582 ) ;
#10863 = VECTOR ( 'NONE', #14178, 1000.000000000000000 ) ;
#10864 = DIRECTION ( 'NONE',  ( -0.1566598588826321747, 0.9876526153536343555, 0.000000000000000000 ) ) ;
#10865 = VECTOR ( 'NONE', #6570, 1000.000000000000000 ) ;
#10866 = ORIENTED_EDGE ( 'NONE', *, *, #3222, .F. ) ;
#10867 = CARTESIAN_POINT ( 'NONE',  ( -47.48906576312474215, -85.48789275826510448, -17.32050807568878525 ) ) ;
#10868 = CIRCLE ( 'NONE', #5130, 2.000000000000001776 ) ;
#10869 = AXIS2_PLACEMENT_3D ( 'NONE', #5032, #17892, #515 ) ;
#10870 = CARTESIAN_POINT ( 'NONE',  ( -74.97862068226375243, -27.08026443497991309, 17.32050807568881723 ) ) ;
#10871 = EDGE_LOOP ( 'NONE', ( #5081, #17152, #1651, #4190 ) ) ;
#10872 = DIRECTION ( 'NONE',  ( -0.1566598588826321747, 0.9876526153536343555, 0.000000000000000000 ) ) ;
#10873 = FACE_OUTER_BOUND ( 'NONE', #9579, .T. ) ;
#10874 = DIRECTION ( 'NONE',  ( -0.1566598588826321192, 0.9876526153536342445, 7.798540720466730171E-17 ) ) ;
#10875 = DIRECTION ( 'NONE',  ( -0.9876526153536336894, -0.1566598588826349503, 0.000000000000000000 ) ) ;
#10876 = B_SPLINE_CURVE_WITH_KNOTS ( 'NONE', 3,
 ( #2248, #8324, #8131, #11143, #3839, #2449, #17064, #15603, #5386, #11327, #8027, #15429, #11246, #1137, #14193, #5580, #13792, #4034 ),
 .UNSPECIFIED., .F., .F.,
 ( 4, 2, 2, 2, 2, 2, 2, 2, 4 ),
 ( 0.1542941748202715790, 0.2407081638136732704, 0.3271221528070749063, 0.4135361418004766532, 0.4999501307938782890, 0.5863641197872799804, 0.6727781087806816718, 0.7591920977740833631, 0.8456060867674841663 ),
 .UNSPECIFIED. ) ;
#10877 = CARTESIAN_POINT ( 'NONE',  ( -126.5488609203928831, -15.30456603905313173, -2.499999999999998668 ) ) ;
#10878 = DIRECTION ( 'NONE',  ( -0.1566598588826321747, 0.9876526153536343555, 0.000000000000000000 ) ) ;
#10879 = AXIS2_PLACEMENT_3D ( 'NONE', #3942, #12655, #5290 ) ;
#10880 = CARTESIAN_POINT ( 'NONE',  ( -5.513829610595458064, -78.82984875575324679, -12.99038105676658539 ) ) ;
#10881 = ADVANCED_FACE ( 'NONE', ( #13398 ), #6418, .F. ) ;
#10882 = EDGE_LOOP ( 'NONE', ( #5510, #11021 ) ) ;
#10883 = AXIS2_PLACEMENT_3D ( 'NONE', #419, #18163, #14038 ) ;
#10884 = EDGE_CURVE ( 'NONE', #9527, #1938, #17268, .T. ) ;
#10885 = CARTESIAN_POINT ( 'NONE',  ( -129.1404785418517918, -2.850701963179326892, -12.74754878398196389 ) ) ;
#10886 = DIRECTION ( 'NONE',  ( -0.9876526153536344665, -0.1566598588826304539, 0.000000000000000000 ) ) ;
#10887 = AXIS2_PLACEMENT_3D ( 'NONE', #4642, #4729, #8997 ) ;
#10888 = CARTESIAN_POINT ( 'NONE',  ( -54.44226908077801852, -28.88533033409541062, -8.660254037844380193 ) ) ;
#10889 = EDGE_LOOP ( 'NONE', ( #9811, #15740 ) ) ;
#10890 = ORIENTED_EDGE ( 'NONE', *, *, #17484, .T. ) ;
#10891 = ORIENTED_EDGE ( 'NONE', *, *, #18720, .F. ) ;
#10892 = CIRCLE ( 'NONE', #10591, 2.500000000000002220 ) ;
#10893 = EDGE_LOOP ( 'NONE', ( #15015, #9842 ) ) ;
#10894 = DIRECTION ( 'NONE',  ( -0.1566598588826321192, 0.9876526153536342445, 7.798540720466730171E-17 ) ) ;
#10895 = AXIS2_PLACEMENT_3D ( 'NONE', #17912, #15122, #7928 ) ;
#10896 = FACE_BOUND ( 'NONE', #17534, .T. ) ;
#10897 = ORIENTED_EDGE ( 'NONE', *, *, #17001, .F. ) ;
#10898 = CIRCLE ( 'NONE', #14849, 1.500000000000001332 ) ;
#10899 = EDGE_LOOP ( 'NONE', ( #18400, #1952 ) ) ;
#10900 = LINE ( 'NONE', #3875, #1290 ) ;
#10901 = AXIS2_PLACEMENT_3D ( 'NONE', #13208, #8770, #10176 ) ;
#10902 = LINE ( 'NONE', #9588, #4538 ) ;
#10904 = FACE_OUTER_BOUND ( 'NONE', #10039, .T. ) ;
#10903 = CIRCLE ( 'NONE', #2767, 1.499999999999999556 ) ;
#10905 = DIRECTION ( 'NONE',  ( 0.000000000000000000, 0.000000000000000000, 1.000000000000000000 ) ) ;
#10906 = CARTESIAN_POINT ( 'NONE',  ( -78.43540483600145308, -27.62857394106911357, -8.660254037844380193 ) ) ;
#10907 = VERTEX_POINT ( 'NONE', #1853 ) ;
#10908 = EDGE_LOOP ( 'NONE', ( #7297, #3996 ) ) ;
#10909 = DIRECTION ( 'NONE',  ( -1.000000000000000000, 0.000000000000000000, 0.000000000000000000 ) ) ;
#10910 = ORIENTED_EDGE ( 'NONE', *, *, #18443, .T. ) ;
#10911 = ADVANCED_FACE ( 'NONE', ( #433 ), #17799, .F. ) ;
#10912 = CARTESIAN_POINT ( 'NONE',  ( -170.2279335768367048, 32.06947484904029011, -4.224609204322613998 ) ) ;
#10913 = VERTEX_POINT ( 'NONE', #15014 ) ;
#10914 = ORIENTED_EDGE ( 'NONE', *, *, #8971, .T. ) ;
#10915 = CYLINDRICAL_SURFACE ( 'NONE', #13043, 1.500000000000000666 ) ;
#10916 = ADVANCED_FACE ( 'NONE', ( #7917 ), #12156, .F. ) ;
#10917 = ORIENTED_EDGE ( 'NONE', *, *, #10140, .F. ) ;
#10918 = ORIENTED_EDGE ( 'NONE', *, *, #12391, .T. ) ;
#10919 = CARTESIAN_POINT ( 'NONE',  ( -69.99999999999998579, -45.00000000000000711, 20.00000000000001776 ) ) ;
#10920 = AXIS2_PLACEMENT_3D ( 'NONE', #12491, #18333, #5301 ) ;
#10921 = CIRCLE ( 'NONE', #2461, 1.500000000000001332 ) ;
#10922 = CARTESIAN_POINT ( 'NONE',  ( -25.80034323552273534, -24.34219442649909126, 12.99038105676661736 ) ) ;
#10923 = EDGE_CURVE ( 'NONE', #15832, #16090, #3588, .T. ) ;
#10924 = CYLINDRICAL_SURFACE ( 'NONE', #13027, 1.500000000000001554 ) ;
#10925 = AXIS2_PLACEMENT_3D ( 'NONE', #13055, #8892, #5953 ) ;
#10926 = DIRECTION ( 'NONE',  ( -0.9876526153536341335, -0.1566598588826327021, 0.000000000000000000 ) ) ;
#10927 = PLANE ( 'NONE',  #6038 ) ;
#10928 =( NAMED_UNIT ( * ) SI_UNIT ( $, .STERADIAN. ) SOLID_ANGLE_UNIT ( ) );
#10929 = VECTOR ( 'NONE', #8659, 1000.000000000000000 ) ;
#10930 = DIRECTION ( 'NONE',  ( -0.1566598588826321192, 0.9876526153536342445, 7.798540720466730171E-17 ) ) ;
#10931 = DIRECTION ( 'NONE',  ( -0.1566598588826321192, 0.9876526153536342445, 7.798540720466731404E-17 ) ) ;
#10932 = AXIS2_PLACEMENT_3D ( 'NONE', #8256, #14019, #12579 ) ;
#10933 = CARTESIAN_POINT ( 'NONE',  ( -38.14600092744311155, -26.30044266253198160, -17.32050807568878170 ) ) ;
#10934 = VERTEX_POINT ( 'NONE', #16254 ) ;
#10935 = ORIENTED_EDGE ( 'NONE', *, *, #17731, .T. ) ;
#10936 = FACE_BOUND ( 'NONE', #16273, .T. ) ;
#10937 = CARTESIAN_POINT ( 'NONE',  ( -1.069392841504132052, -78.12487939078141608, -17.32050807568878525 ) ) ;
#10938 = EDGE_LOOP ( 'NONE', ( #9843, #5394, #11288, #302 ) ) ;
#10939 = EDGE_CURVE ( 'NONE', #13454, #6106, #911, .T. ) ;
#10940 = DIRECTION ( 'NONE',  ( -0.9876526153536336894, -0.1566598588826349503, 0.000000000000000000 ) ) ;
#10941 = EDGE_LOOP ( 'NONE', ( #15858, #11306 ) ) ;
#10942 = CARTESIAN_POINT ( 'NONE',  ( -68.55887868246516348, -26.06197535224279704, -8.660254037844380193 ) ) ;
#10943 = DIRECTION ( 'NONE',  ( -0.1566598588826321192, 0.9876526153536342445, 7.798540720466730171E-17 ) ) ;
#10944 = EDGE_CURVE ( 'NONE', #3259, #5362, #9015, .T. ) ;
#10945 = CARTESIAN_POINT ( 'NONE',  ( -19.34096622554629263, -81.02308678011010556, 1.424741226644455312E-14 ) ) ;
#10946 = DIRECTION ( 'NONE',  ( 0.000000000000000000, 0.000000000000000000, 1.000000000000000000 ) ) ;
#10947 = EDGE_LOOP ( 'NONE', ( #8244, #8854 ) ) ;
#10948 = CIRCLE ( 'NONE', #2182, 1.500000000000001332 ) ;
#10949 = DIRECTION ( 'NONE',  ( -0.9876526153536336894, -0.1566598588826349503, 0.000000000000000000 ) ) ;
#10950 = CARTESIAN_POINT ( 'NONE',  ( -69.54653129781877396, -26.21863521112543083, -12.99038105676658006 ) ) ;
#10951 = DIRECTION ( 'NONE',  ( 0.000000000000000000, 0.000000000000000000, 1.000000000000000000 ) ) ;
#10952 =( LENGTH_UNIT ( ) NAMED_UNIT ( * ) SI_UNIT ( .MILLI., .METRE. ) );
#10953 = EDGE_CURVE ( 'NONE', #10686, #1614, #15421, .T. ) ;
#10954 = MECHANICAL_DESIGN_GEOMETRIC_PRESENTATION_REPRESENTATION (  '', ( #388 ), #87 ) ;
#10955 = DIRECTION ( 'NONE',  ( -0.000000000000000000, -0.000000000000000000, -1.000000000000000000 ) ) ;
#10956 = DIRECTION ( 'NONE',  ( -0.9876526153536336894, -0.1566598588826350336, 0.000000000000000000 ) ) ;
#10957 = CARTESIAN_POINT ( 'NONE',  ( 7.819480696678551723, -76.71494066083772623, -4.330127018922189208 ) ) ;
#10958 = DIRECTION ( 'NONE',  ( -0.1566598588826321192, 0.9876526153536342445, 7.798540720466731404E-17 ) ) ;
#10959 = ORIENTED_EDGE ( 'NONE', *, *, #10745, .T. ) ;
#10960 = ORIENTED_EDGE ( 'NONE', *, *, #13853, .T. ) ;
#10961 = CYLINDRICAL_SURFACE ( 'NONE', #17487, 1.500000000000000666 ) ;
#10962 = ORIENTED_EDGE ( 'NONE', *, *, #13737, .T. ) ;
#10963 = AXIS2_PLACEMENT_3D ( 'NONE', #13357, #6177, #11905 ) ;
#10964 = ADVANCED_FACE ( 'NONE', ( #530, #9431, #9615 ), #10927, .F. ) ;
#10965 = DIRECTION ( 'NONE',  ( 0.1856185419698762329, -0.9826218788918640312, 0.000000000000000000 ) ) ;
#10966 = DIRECTION ( 'NONE',  ( 0.000000000000000000, 0.000000000000000000, 1.000000000000000000 ) ) ;
#10967 = CYLINDRICAL_SURFACE ( 'NONE', #6539, 1.500000000000001554 ) ;
#10968 = CARTESIAN_POINT ( 'NONE',  ( -46.54104815794895700, -27.63205146303434390, -8.660254037844380193 ) ) ;
#10969 = DIRECTION ( 'NONE',  ( -0.1566598588826321747, 0.9876526153536343555, 0.000000000000000000 ) ) ;
#10970 = EDGE_CURVE ( 'NONE', #5711, #10784, #13968, .T. ) ;
#10971 = CARTESIAN_POINT ( 'NONE',  ( -129.0032285637105360, -14.74502811105983469, -4.582591203971078997 ) ) ;
#10972 = DIRECTION ( 'NONE',  ( -0.9876526153536341335, -0.1566598588826327576, 0.000000000000000000 ) ) ;
#10973 = FACE_OUTER_BOUND ( 'NONE', #15213, .T. ) ;
#10974 = CARTESIAN_POINT ( 'NONE',  ( -49.50400600400987372, -28.10203103968224170, -17.32050807568878170 ) ) ;
#10975 = ORIENTED_EDGE ( 'NONE', *, *, #16669, .T. ) ;
#10976 = FACE_BOUND ( 'NONE', #18329, .T. ) ;
#10977 = CARTESIAN_POINT ( 'NONE',  ( -9.299721761247353058, -16.66238381928489787, -8.660254037844380193 ) ) ;
#10978 = AXIS2_PLACEMENT_3D ( 'NONE', #9255, #14944, #10305 ) ;
#10979 = DIRECTION ( 'NONE',  ( -0.1566598588826321192, 0.9876526153536342445, 7.798540720466730171E-17 ) ) ;
#10980 = ORIENTED_EDGE ( 'NONE', *, *, #11760, .F. ) ;
#10981 = ORIENTED_EDGE ( 'NONE', *, *, #872, .T. ) ;
#10982 = CYLINDRICAL_SURFACE ( 'NONE', #8371, 1.500000000000000666 ) ;
#10983 = FACE_BOUND ( 'NONE', #13344, .T. ) ;
#10984 = EDGE_CURVE ( 'NONE', #2681, #12551, #10850, .T. ) ;
#10985 = EDGE_CURVE ( 'NONE', #9759, #4810, #6881, .T. ) ;
#10986 = AXIS2_PLACEMENT_3D ( 'NONE', #12176, #16776, #6721 ) ;
#10987 = EDGE_CURVE ( 'NONE', #8469, #6106, #12451, .T. ) ;
#10988 =( NAMED_UNIT ( * ) PLANE_ANGLE_UNIT ( ) SI_UNIT ( $, .RADIAN. ) );
#10989 = ORIENTED_EDGE ( 'NONE', *, *, #1882, .F. ) ;
#10990 = EDGE_CURVE ( 'NONE', #7954, #15891, #5632, .T. ) ;
#10991 = CARTESIAN_POINT ( 'NONE',  ( -22.63303206852135929, -18.77729191420043264, 1.926565525561698076E-14 ) ) ;
#10992 = DIRECTION ( 'NONE',  ( 0.000000000000000000, 0.000000000000000000, 1.000000000000000000 ) ) ;
#10993 = CARTESIAN_POINT ( 'NONE',  ( -15.92381708198643153, -22.77559583767277473, 21.65063509461101177 ) ) ;
#10994 = ORIENTED_EDGE ( 'NONE', *, *, #8703, .F. ) ;
#10995 = DIRECTION ( 'NONE',  ( 0.9201637183752248150, -0.3915338189555022108, 0.000000000000000000 ) ) ;
#10996 = DIRECTION ( 'NONE',  ( -0.9876526153536341335, -0.1566598588826327021, 0.000000000000000000 ) ) ;
#10997 = ORIENTED_EDGE ( 'NONE', *, *, #8118, .F. ) ;
#10998 = DIRECTION ( 'NONE',  ( 0.000000000000000000, 0.000000000000000000, 1.000000000000000000 ) ) ;
#10999 = CYLINDRICAL_SURFACE ( 'NONE', #15753, 1.500000000000001554 ) ;
#11000 = DIRECTION ( 'NONE',  ( -0.1566598588826321192, 0.9876526153536342445, 7.798540720466730171E-17 ) ) ;
#11001 = ORIENTED_EDGE ( 'NONE', *, *, #17194, .T. ) ;
#11002 = EDGE_LOOP ( 'NONE', ( #5514, #13361, #2419, #12392 ) ) ;
#11003 = CARTESIAN_POINT ( 'NONE',  ( -44.03228160938703439, -84.93958325217590755, 8.660254037844412167 ) ) ;
#11004 = ORIENTED_EDGE ( 'NONE', *, *, #9806, .F. ) ;
#11005 = LINE ( 'NONE', #10919, #12733 ) ;
#11006 = EDGE_CURVE ( 'NONE', #17992, #3563, #3802, .T. ) ;
#11007 = DIRECTION ( 'NONE',  ( -0.9876526153536341335, -0.1566598588826327021, 0.000000000000000000 ) ) ;
#11008 = EDGE_CURVE ( 'NONE', #6102, #3468, #10822, .T. ) ;
#11009 = CARTESIAN_POINT ( 'NONE',  ( -50.28730529842302843, -23.16376796291410756, -17.32050807568878170 ) ) ;
#11010 = CARTESIAN_POINT ( 'NONE',  ( -51.27495791377664602, -23.32042782179674134, -12.99038105676658006 ) ) ;
#11011 = CARTESIAN_POINT ( 'NONE',  ( -70.23909404122630917, 45.10173559463541437, 5.879686486593318939 ) ) ;
#11012 = CARTESIAN_POINT ( 'NONE',  ( -70.00000000000000000, 44.99999999999999289, 25.00000000000000000 ) ) ;
#11013 = CARTESIAN_POINT ( 'NONE',  ( 0.000000000000000000, 0.000000000000000000, 0.000000000000000000 ) ) ;
#11014 = EDGE_CURVE ( 'NONE', #98, #8230, #18080, .T. ) ;
#11015 = DIRECTION ( 'NONE',  ( -0.1566598588826321192, 0.9876526153536342445, 7.798540720466730171E-17 ) ) ;
#11016 = CIRCLE ( 'NONE', #11910, 1.500000000000000888 ) ;
#11017 = CARTESIAN_POINT ( 'NONE',  ( -47.81817376003893827, -22.77211831570753020, -12.99038105676658006 ) ) ;
#11018 = CARTESIAN_POINT ( 'NONE',  ( -58.84707083969148300, -87.28948113541537168, 17.32050807568881368 ) ) ;
#11019 = CARTESIAN_POINT ( 'NONE',  ( -35.47251606811855851, -20.81387007967463987, 1.908195823574487804E-14 ) ) ;
#11020 = VERTEX_POINT ( 'NONE', #18479 ) ;
#11021 = ORIENTED_EDGE ( 'NONE', *, *, #15973, .F. ) ;
#11022 = CARTESIAN_POINT ( 'NONE',  ( -59.38053215754616332, -29.66862962850856533, 1.869203119972154228E-14 ) ) ;
#11023 = DIRECTION ( 'NONE',  ( -0.9876526153536336894, -0.1566598588826350336, 0.000000000000000000 ) ) ;
#11024 = ORIENTED_EDGE ( 'NONE', *, *, #7408, .F. ) ;
#11025 = LINE ( 'NONE', #6798, #12395 ) ;
#11026 = ORIENTED_EDGE ( 'NONE', *, *, #2998, .T. ) ;
#11027 = EDGE_LOOP ( 'NONE', ( #15877, #7323, #12649, #18033 ) ) ;
#11028 = CYLINDRICAL_SURFACE ( 'NONE', #3948, 1.500000000000001554 ) ;
#11029 = FACE_OUTER_BOUND ( 'NONE', #8320, .T. ) ;
#11030 = ORIENTED_EDGE ( 'NONE', *, *, #7944, .F. ) ;
#11031 = AXIS2_PLACEMENT_3D ( 'NONE', #9161, #10564, #12160 ) ;
#11032 = CARTESIAN_POINT ( 'NONE',  ( -61.84966369593023217, -30.06027927571513914, 12.99038105676661736 ) ) ;
#11033 = DIRECTION ( 'NONE',  ( -0.1566598588826321747, 0.9876526153536343555, 0.000000000000000000 ) ) ;
#11034 = CARTESIAN_POINT ( 'NONE',  ( -26.78799585087635649, -24.49885428538171794, 17.32050807568881723 ) ) ;
#11035 = ORIENTED_EDGE ( 'NONE', *, *, #11898, .F. ) ;
#11036 = CARTESIAN_POINT ( 'NONE',  ( -12.75650591498505371, -17.21069332537411256, 8.660254037844413944 ) ) ;
#11037 = SHAPE_REPRESENTATION_RELATIONSHIP ( 'NONE' , 'NONE' ,  #5397, #10448 ) ;
#11038 = EDGE_CURVE ( 'NONE', #6863, #4996, #6621, .T. ) ;
#11039 = B_SPLINE_CURVE_WITH_KNOTS ( 'NONE', 3,
 ( #4235, #5291, #2626, #8413, #9917, #15815, #14387, #9654, #4128, #15523, #14095, #18616 ),
 .UNSPECIFIED., .F., .F.,
 ( 4, 2, 2, 2, 2, 4 ),
 ( -1.414213904430124076E-05, 0.001573093992944416377, 0.003160330124933133974, 0.003953948190927493098, 0.004747566256921851788, 0.006334802388910591719 ),
 .UNSPECIFIED. ) ;
#11040 = ORIENTED_EDGE ( 'NONE', *, *, #13483, .T. ) ;
#11041 = PRODUCT_DEFINITION_SHAPE ( 'NONE', 'NONE',  #9414 ) ;
#11042 = EDGE_CURVE ( 'NONE', #4036, #7437, #13547, .T. ) ;
#11043 = DIRECTION ( 'NONE',  ( 0.000000000000000000, 0.000000000000000000, 1.000000000000000000 ) ) ;
#11044 = ORIENTED_EDGE ( 'NONE', *, *, #13511, .F. ) ;
#11045 = DIRECTION ( 'NONE',  ( -0.1566598588826321192, 0.9876526153536342445, 7.798540720466730171E-17 ) ) ;
#11046 = DIRECTION ( 'NONE',  ( -0.1566598588826321747, 0.9876526153536343555, 0.000000000000000000 ) ) ;
#11047 = ORIENTED_EDGE ( 'NONE', *, *, #11070, .T. ) ;
#11048 = CARTESIAN_POINT ( 'NONE',  ( -10.45209268736360997, -79.61314805016641571, 21.65063509461100821 ) ) ;
#11049 = EDGE_CURVE ( 'NONE', #2279, #13719, #3857, .T. ) ;
#11050 = AXIS2_PLACEMENT_3D ( 'NONE', #6111, #7628, #9220 ) ;
#11051 = LINE ( 'NONE', #14005, #12924 ) ;
#11052 = ORIENTED_EDGE ( 'NONE', *, *, #18353, .T. ) ;
#11053 = CARTESIAN_POINT ( 'NONE',  ( -40.61513246582717329, -26.69209230973856251, -4.330127018922181215 ) ) ;
#11054 = ORIENTED_EDGE ( 'NONE', *, *, #1067, .T. ) ;
#11055 = EDGE_LOOP ( 'NONE', ( #18177, #18169, #8654, #7788 ) ) ;
#11056 = AXIS2_PLACEMENT_3D ( 'NONE', #14020, #9382, #15249 ) ;
#11057 = EDGE_LOOP ( 'NONE', ( #13409, #6931, #1600, #13404 ) ) ;
#11058 = DIRECTION ( 'NONE',  ( -0.1566598588826321192, 0.9876526153536342445, 7.798540720466731404E-17 ) ) ;
#11059 = ORIENTED_EDGE ( 'NONE', *, *, #7949, .F. ) ;
#11060 = CARTESIAN_POINT ( 'NONE',  ( -5.842937607509656850, -16.11407431319567962, 8.660254037844412167 ) ) ;
#11061 = CARTESIAN_POINT ( 'NONE',  ( -60.36818477289977380, -29.82528948739119556, 12.99038105676661736 ) ) ;
#11062 = DIRECTION ( 'NONE',  ( 1.000000000000000000, 0.000000000000000000, 0.000000000000000000 ) ) ;
#11063 = DIRECTION ( 'NONE',  ( -0.1566598588826321192, 0.9876526153536342445, 7.798540720466731404E-17 ) ) ;
#11064 = DIRECTION ( 'NONE',  ( -0.9201637183752250371, 0.3915338189555017112, -0.000000000000000000 ) ) ;
#11065 = CARTESIAN_POINT ( 'NONE',  ( -127.5060788346647485, 9.551739887561357278, -2.821239268406352085 ) ) ;
#11066 = DIRECTION ( 'NONE',  ( -0.1566598588826321747, 0.9876526153536343555, 0.000000000000000000 ) ) ;
#11067 = FACE_BOUND ( 'NONE', #16470, .T. ) ;
#11068 = DIRECTION ( 'NONE',  ( -0.1566598588826321192, 0.9876526153536342445, 7.798540720466731404E-17 ) ) ;
#11069 = CIRCLE ( 'NONE', #17462, 2.000000000000000000 ) ;
#11070 = EDGE_CURVE ( 'NONE', #16672, #1209, #18188, .T. ) ;
#11071 = LINE ( 'NONE', #7629, #14733 ) ;
#11072 = DIRECTION ( 'NONE',  ( -0.1566598588826321192, 0.9876526153536342445, 7.798540720466731404E-17 ) ) ;
#11073 = EDGE_LOOP ( 'NONE', ( #7884, #4911, #17383, #4585 ) ) ;
#11074 = CIRCLE ( 'NONE', #16549, 1.500000000000001332 ) ;
#11075 = ORIENTED_EDGE ( 'NONE', *, *, #13168, .F. ) ;
#11076 = EDGE_CURVE ( 'NONE', #8123, #14703, #4775, .T. ) ;
#11077 = ORIENTED_EDGE ( 'NONE', *, *, #10531, .F. ) ;
#11078 = CARTESIAN_POINT ( 'NONE',  ( -90.00000000000000000, 34.99999999999999289, 100.5765140304660861 ) ) ;
#11079 = ORIENTED_EDGE ( 'NONE', *, *, #17095, .T. ) ;
#11080 = FACE_BOUND ( 'NONE', #10889, .T. ) ;
#11081 = AXIS2_PLACEMENT_3D ( 'NONE', #12975, #15921, #18726 ) ;
#11082 = EDGE_LOOP ( 'NONE', ( #5973, #16763, #17693, #15671 ) ) ;
#11083 = AXIS2_PLACEMENT_3D ( 'NONE', #7548, #10563, #3257 ) ;
#11084 = CARTESIAN_POINT ( 'NONE',  ( -48.02252708097942246, -27.86704125135829813, -17.32050807568878170 ) ) ;
#11085 = AXIS2_PLACEMENT_3D ( 'NONE', #6070, #7401, #16012 ) ;
#11086 = DIRECTION ( 'NONE',  ( -0.9539392014169441047, -0.3000000000000045963, 0.000000000000000000 ) ) ;
#11087 = FACE_OUTER_BOUND ( 'NONE', #3121, .T. ) ;
#11088 = VECTOR ( 'NONE', #14940, 1000.000000000000000 ) ;
#11089 = DIRECTION ( 'NONE',  ( -0.1566598588826321192, 0.9876526153536342445, 7.798540720466731404E-17 ) ) ;
#11090 = DIRECTION ( 'NONE',  ( -0.1566598588826321192, 0.9876526153536342445, 7.798540720466730171E-17 ) ) ;
#11091 = ADVANCED_FACE ( 'NONE', ( #9520 ), #9982, .T. ) ;
#11092 = VERTEX_POINT ( 'NONE', #16213 ) ;
#11093 = DIRECTION ( 'NONE',  ( -0.9876526153536336894, -0.1566598588826350336, 0.000000000000000000 ) ) ;
#11094 = EDGE_CURVE ( 'NONE', #3775, #8040, #15388, .T. ) ;
#11095 = DIRECTION ( 'NONE',  ( -0.9876526153536336894, -0.1566598588826349503, 0.000000000000000000 ) ) ;
#11096 = EDGE_CURVE ( 'NONE', #15378, #14170, #4641, .T. ) ;
#11097 = DIRECTION ( 'NONE',  ( 1.438274729681541867E-16, 6.252920376642369977E-17, -1.000000000000000000 ) ) ;
#11098 = EDGE_LOOP ( 'NONE', ( #5559, #14389, #7464, #3512 ) ) ;
#11099 = ORIENTED_EDGE ( 'NONE', *, *, #1612, .T. ) ;
#11100 = DIRECTION ( 'NONE',  ( -0.1566598588826321192, 0.9876526153536342445, 7.798540720466730171E-17 ) ) ;
#11101 = CIRCLE ( 'NONE', #18732, 1.500000000000000888 ) ;
#11102 = VERTEX_POINT ( 'NONE', #11481 ) ;
#11103 = ORIENTED_EDGE ( 'NONE', *, *, #13132, .F. ) ;
#11104 = CARTESIAN_POINT ( 'NONE',  ( -126.5450966053943631, -15.30041110265608673, 2.520603730400377884 ) ) ;
#11105 = CIRCLE ( 'NONE', #2937, 1.500000000000001332 ) ;
#11106 = CIRCLE ( 'NONE', #3231, 15.83618137761393463 ) ;
#11107 = FACE_OUTER_BOUND ( 'NONE', #11351, .T. ) ;
#11108 = CARTESIAN_POINT ( 'NONE',  ( -33.16810284049712010, -83.21632480446695013, -12.99038105676658539 ) ) ;
#11109 = CYLINDRICAL_SURFACE ( 'NONE', #2730, 1.500000000000001554 ) ;
#11110 = CARTESIAN_POINT ( 'NONE',  ( -127.1404785156000941, -15.31509901360656478, -2.500000000000000000 ) ) ;
#11111 = CARTESIAN_POINT ( 'NONE',  ( 0.000000000000000000, 0.000000000000000000, 37.00000000000000711 ) ) ;
#11112 = VECTOR ( 'NONE', #16800, 1000.000000000000000 ) ;
#11113 = DIRECTION ( 'NONE',  ( -0.1566598588826321747, 0.9876526153536343555, 0.000000000000000000 ) ) ;
#11114 = DIRECTION ( 'NONE',  ( -0.1566598588826321747, 0.9876526153536343555, 0.000000000000000000 ) ) ;
#11115 = EDGE_CURVE ( 'NONE', #1326, #1662, #7519, .T. ) ;
#11116 = EDGE_LOOP ( 'NONE', ( #12627, #4694, #12384, #9065 ) ) ;
#11117 = ORIENTED_EDGE ( 'NONE', *, *, #13796, .F. ) ;
#11118 = FACE_BOUND ( 'NONE', #6903, .T. ) ;
#11119 = DIRECTION ( 'NONE',  ( -0.1566598588826321192, 0.9876526153536342445, 7.798540720466730171E-17 ) ) ;
#11120 = EDGE_LOOP ( 'NONE', ( #4905, #15283, #8471, #13688 ) ) ;
#11121 = ORIENTED_EDGE ( 'NONE', *, *, #3055, .T. ) ;
#11122 = EDGE_CURVE ( 'NONE', #8055, #13293, #7596, .T. ) ;
#11123 = ORIENTED_EDGE ( 'NONE', *, *, #14249, .T. ) ;
#11124 = VECTOR ( 'NONE', #844, 1000.000000000000000 ) ;
#11125 = CARTESIAN_POINT ( 'NONE',  ( -1.109027851681966492, -20.42569795443330349, -12.99038105676658361 ) ) ;
#11126 = VERTEX_POINT ( 'NONE', #16305 ) ;
#11127 = DIRECTION ( 'NONE',  ( -0.1566598588826321192, 0.9876526153536342445, 7.798540720466731404E-17 ) ) ;
#11128 = VECTOR ( 'NONE', #14970, 1000.000000000000000 ) ;
#11129 = AXIS2_PLACEMENT_3D ( 'NONE', #11328, #1236, #7198 ) ;
#11130 = DIRECTION ( 'NONE',  ( -0.1566598588826321192, 0.9876526153536342445, 7.798540720466730171E-17 ) ) ;
#11131 = CIRCLE ( 'NONE', #2675, 2.000000000000000000 ) ;
#11132 = EDGE_LOOP ( 'NONE', ( #97, #1945 ) ) ;
#11133 = CARTESIAN_POINT ( 'NONE',  ( -57.36559191666103175, -87.05449134709141390, -17.32050807568878525 ) ) ;
#11134 = DIRECTION ( 'NONE',  ( -0.1566598588826321192, 0.9876526153536342445, 7.798540720466730171E-17 ) ) ;
#11135 = CARTESIAN_POINT ( 'NONE',  ( 0.000000000000000000, 0.000000000000000000, 0.000000000000000000 ) ) ;
#11136 = CYLINDRICAL_SURFACE ( 'NONE', #12984, 1.500000000000001554 ) ;
#11137 = ORIENTED_EDGE ( 'NONE', *, *, #11680, .T. ) ;
#11139 = CARTESIAN_POINT ( 'NONE',  ( -9.997901389864651378, -21.83563668437698269, -8.660254037844380193 ) ) ;
#11138 = VECTOR ( 'NONE', #16159, 1000.000000000000000 ) ;
#11140 = CIRCLE ( 'NONE', #2380, 1.500000000000001332 ) ;
#11141 = DIRECTION ( 'NONE',  ( -0.9876526153536341335, -0.1566598588826327021, 0.000000000000000000 ) ) ;
#11142 = ORIENTED_EDGE ( 'NONE', *, *, #8959, .T. ) ;
#11143 = CARTESIAN_POINT ( 'NONE',  ( -83.85307456958885552, 31.66350799028677798, 35.00001200000000523 ) ) ;
#11144 = CIRCLE ( 'NONE', #13559, 1.500000000000000888 ) ;
#11145 = CARTESIAN_POINT ( 'NONE',  ( -71.90911978745813826, 1.387778780781445676E-14, 110.7545852194966045 ) ) ;
#11147 = ORIENTED_EDGE ( 'NONE', *, *, #6843, .T. ) ;
#11146 = LINE ( 'NONE', #18228, #17856 ) ;
#11148 = ORIENTED_EDGE ( 'NONE', *, *, #6359, .F. ) ;
#11149 = CARTESIAN_POINT ( 'NONE',  ( 7.819480696678551723, -76.71494066083772623, 4.330127018922207860 ) ) ;
#11150 = VERTEX_POINT ( 'NONE', #7161 ) ;
#11151 = EDGE_CURVE ( 'NONE', #10291, #15850, #18580, .T. ) ;
#11152 = ORIENTED_EDGE ( 'NONE', *, *, #9495, .T. ) ;
#11153 = ADVANCED_FACE ( 'NONE', ( #1380 ), #3300, .F. ) ;
#11154 = VECTOR ( 'NONE', #15936, 1000.000000000000114 ) ;
#11155 = DIRECTION ( 'NONE',  ( -1.000000000000000000, 0.000000000000000000, 0.000000000000000000 ) ) ;
#11156 = EDGE_CURVE ( 'NONE', #8290, #11838, #13008, .T. ) ;
#11157 = DIRECTION ( 'NONE',  ( -0.9876526153536336894, -0.1566598588826349503, 0.000000000000000000 ) ) ;
#11158 = AXIS2_PLACEMENT_3D ( 'NONE', #5202, #12383, #9361 ) ;
#11159 = DIRECTION ( 'NONE',  ( 8.693966348389027220E-17, -1.991237296706374949E-16, 1.000000000000000000 ) ) ;
#11160 = CARTESIAN_POINT ( 'NONE',  ( -168.4538323585589694, 31.95594125380572947, -2.500000000000000000 ) ) ;
#11161 = DIRECTION ( 'NONE',  ( -0.9876526153536336894, -0.1566598588826349503, 0.000000000000000000 ) ) ;
#11162 = ORIENTED_EDGE ( 'NONE', *, *, #6828, .T. ) ;
#11163 = CARTESIAN_POINT ( 'NONE',  ( -72.50948914387967648, -26.68861478777333573, 21.65063509461101887 ) ) ;
#11164 = FACE_BOUND ( 'NONE', #16785, .T. ) ;
#11165 = AXIS2_PLACEMENT_3D ( 'NONE', #10922, #2399, #8194 ) ;
#11166 = DIRECTION ( 'NONE',  ( -0.1566598588826321192, 0.9876526153536342445, 7.798540720466730171E-17 ) ) ;
#11167 = AXIS2_PLACEMENT_3D ( 'NONE', #14887, #1909, #488 ) ;
#11168 = DIRECTION ( 'NONE',  ( -0.9876526153536336894, -0.1566598588826349503, 0.000000000000000000 ) ) ;
#11169 = AXIS2_PLACEMENT_3D ( 'NONE', #14112, #7043, #15623 ) ;
#11170 = ORIENTED_EDGE ( 'NONE', *, *, #14835, .T. ) ;
#11171 = VERTEX_POINT ( 'NONE', #14783 ) ;
#11172 = VERTEX_POINT ( 'NONE', #8581 ) ;
#11173 = EDGE_LOOP ( 'NONE', ( #6140, #11200, #16051, #5335 ) ) ;
#11174 = CYLINDRICAL_SURFACE ( 'NONE', #10168, 2.500000000000002220 ) ;
#11175 = FACE_BOUND ( 'NONE', #7489, .T. ) ;
#11176 = VECTOR ( 'NONE', #6936, 1000.000000000000000 ) ;
#11177 = ADVANCED_FACE ( 'NONE', ( #11299 ), #17115, .F. ) ;
#11178 = CARTESIAN_POINT ( 'NONE',  ( -69.99999999999998579, -45.00000000000000711, 25.00000000000000000 ) ) ;
#11179 = AXIS2_PLACEMENT_3D ( 'NONE', #14906, #7523, #5914 ) ;
#11180 = VERTEX_POINT ( 'NONE', #10417 ) ;
#11181 = AXIS2_PLACEMENT_3D ( 'NONE', #13558, #1731, #11929 ) ;
#11182 = VECTOR ( 'NONE', #9642, 1000.000000000000000 ) ;
#11183 = VERTEX_POINT ( 'NONE', #15777 ) ;
#11184 = DIRECTION ( 'NONE',  ( -0.1566598588826321192, 0.9876526153536342445, 7.798540720466731404E-17 ) ) ;
#11185 = EDGE_CURVE ( 'NONE', #13999, #6818, #3264, .T. ) ;
#11186 = CARTESIAN_POINT ( 'NONE',  ( -10.94591899504043830, -79.69147797960773971, 1.424741226644455312E-14 ) ) ;
#11187 = DIRECTION ( 'NONE',  ( 0.000000000000000000, 0.000000000000000000, -1.000000000000000000 ) ) ;
#11188 = FACE_OUTER_BOUND ( 'NONE', #3141, .T. ) ;
#11189 = CARTESIAN_POINT ( 'NONE',  ( -45.55339554259532520, -27.47539160415171722, 21.65063509461101887 ) ) ;
#11190 = AXIS2_PLACEMENT_3D ( 'NONE', #12658, #11334, #17154 ) ;
#11191 = CARTESIAN_POINT ( 'NONE',  ( -2.057045456857756971, -78.28153924966404986, 12.99038105676660848 ) ) ;
#11192 = AXIS2_PLACEMENT_3D ( 'NONE', #8464, #1450, #10059 ) ;
#11193 = EDGE_LOOP ( 'NONE', ( #8153, #16270 ) ) ;
#11194 = ORIENTED_EDGE ( 'NONE', *, *, #2847, .T. ) ;
#11195 = EDGE_LOOP ( 'NONE', ( #7497, #13351, #16040 ) ) ;
#11196 = VECTOR ( 'NONE', #15844, 1000.000000000000000 ) ;
#11197 = CARTESIAN_POINT ( 'NONE',  ( -58.88670584986932965, -29.59029969906724844, -12.99038105676658006 ) ) ;
#11198 = ORIENTED_EDGE ( 'NONE', *, *, #5339, .T. ) ;
#11199 = ORIENTED_EDGE ( 'NONE', *, *, #12501, .T. ) ;
#11200 = ORIENTED_EDGE ( 'NONE', *, *, #9875, .F. ) ;
#11201 = DIRECTION ( 'NONE',  ( -0.9876526153536341335, -0.1566598588826327021, 0.000000000000000000 ) ) ;
#11202 = EDGE_CURVE ( 'NONE', #7608, #344, #1470, .T. ) ;
#11203 = DIRECTION ( 'NONE',  ( -0.9876526153536341335, -0.1566598588826327021, 0.000000000000000000 ) ) ;
#11204 = VERTEX_POINT ( 'NONE', #2690 ) ;
#11205 = PRODUCT_DEFINITION_SHAPE ( 'NONE', 'NONE',  #12169 ) ;
#11206 = ADVANCED_FACE ( 'NONE', ( #8996 ), #15371, .F. ) ;
#11207 = AXIS2_PLACEMENT_3D ( 'NONE', #7368, #2977, #17421 ) ;
#11208 = VECTOR ( 'NONE', #441, 1000.000000000000000 ) ;
#11209 = DIRECTION ( 'NONE',  ( -0.1566598588826321747, 0.9876526153536343555, 0.000000000000000000 ) ) ;
#11210 = DIRECTION ( 'NONE',  ( -0.000000000000000000, -0.000000000000000000, -1.000000000000000000 ) ) ;
#11211 = EDGE_CURVE ( 'NONE', #5059, #2873, #4182, .T. ) ;
#11212 = DIRECTION ( 'NONE',  ( -1.000000000000000000, 0.000000000000000000, 0.000000000000000000 ) ) ;
#11213 =( NAMED_UNIT ( * ) SI_UNIT ( $, .STERADIAN. ) SOLID_ANGLE_UNIT ( ) );
#11214 = CARTESIAN_POINT ( 'NONE',  ( -25.80034323552273179, -24.34219442649909126, -21.65063509461098334 ) ) ;
#11215 = CIRCLE ( 'NONE', #5171, 1.500000000000001332 ) ;
#11216 = DIRECTION ( 'NONE',  ( -0.1566598588826321192, 0.9876526153536342445, 7.798540720466731404E-17 ) ) ;
#11217 = ORIENTED_EDGE ( 'NONE', *, *, #7277, .T. ) ;
#11218 = ORIENTED_EDGE ( 'NONE', *, *, #7688, .T. ) ;
#11219 = FACE_BOUND ( 'NONE', #3766, .T. ) ;
#11220 = CARTESIAN_POINT ( 'NONE',  ( -72.71384246482016067, -31.78353772342409300, 1.869203119972154228E-14 ) ) ;
#11221 = ORIENTED_EDGE ( 'NONE', *, *, #12545, .F. ) ;
#11222 = VECTOR ( 'NONE', #4140, 1000.000000000000000 ) ;
#11223 = DIRECTION ( 'NONE',  ( -0.1566598588826321192, 0.9876526153536342445, 7.798540720466730171E-17 ) ) ;
#11224 = CARTESIAN_POINT ( 'NONE',  ( -51.43967622453925514, -86.11453219379563961, 21.65063509461101532 ) ) ;
#11225 = ORIENTED_EDGE ( 'NONE', *, *, #8870, .F. ) ;
#11226 = CYLINDRICAL_SURFACE ( 'NONE', #13639, 2.000000000000000000 ) ;
#11227 = EDGE_CURVE ( 'NONE', #17592, #306, #6001, .T. ) ;
#11228 = AXIS2_PLACEMENT_3D ( 'NONE', #11473, #1371, #10249 ) ;
#11229 = CARTESIAN_POINT ( 'NONE',  ( -71.02801022084922522, -26.45362499944938151, 4.330127018922218518 ) ) ;
#11230 = EDGE_CURVE ( 'NONE', #15425, #16044, #15987, .T. ) ;
#11231 = AXIS2_PLACEMENT_3D ( 'NONE', #6976, #5542, #11295 ) ;
#11232 = ORIENTED_EDGE ( 'NONE', *, *, #3929, .T. ) ;
#11233 = EDGE_CURVE ( 'NONE', #14533, #2476, #4197, .T. ) ;
#11234 = CARTESIAN_POINT ( 'NONE',  ( -129.1404785418517918, 8.649298036820676217, 5.500000000000000000 ) ) ;
#11235 = ADVANCED_FACE ( 'NONE', ( #3574 ), #16801, .F. ) ;
#11236 = FACE_OUTER_BOUND ( 'NONE', #1288, .T. ) ;
#11237 = CARTESIAN_POINT ( 'NONE',  ( 5.000000000000000000, 6.123233995736766282E-16, -35.00000000000000000 ) ) ;
#11238 = SURFACE_STYLE_FILL_AREA ( #18106 ) ;
#11239 = CIRCLE ( 'NONE', #3667, 1.500000000000000444 ) ;
#11240 = DIRECTION ( 'NONE',  ( -0.1566598588826321192, 0.9876526153536342445, 7.798540720466730171E-17 ) ) ;
#11241 = DIRECTION ( 'NONE',  ( -0.1566598588826321192, 0.9876526153536342445, 7.798540720466731404E-17 ) ) ;
#11242 = CARTESIAN_POINT ( 'NONE',  ( -172.0951522251743029, 56.61964399677355431, -2.500000000000000000 ) ) ;
#11243 = CARTESIAN_POINT ( 'NONE',  ( -73.70149508017377116, -31.94019758230671258, 4.330127018922217630 ) ) ;
#11244 = EDGE_LOOP ( 'NONE', ( #3109, #7969, #5927, #17247 ) ) ;
#11245 = AXIS2_PLACEMENT_3D ( 'NONE', #16697, #4725, #4821 ) ;
#11246 = CARTESIAN_POINT ( 'NONE',  ( -80.84224302102266790, 30.66666482925224102, 35.00001199999999812 ) ) ;
#11247 = CARTESIAN_POINT ( 'NONE',  ( -34.19539046602857724, -25.67380322700145356, 21.65063509461101887 ) ) ;
#11249 = EDGE_LOOP ( 'NONE', ( #17029, #17655, #16873, #869 ) ) ;
#11248 = DIRECTION ( 'NONE',  ( -0.1566598588826321192, 0.9876526153536342445, 7.798540720466731404E-17 ) ) ;
#11250 = VERTEX_POINT ( 'NONE', #9477 ) ;
#11251 = ORIENTED_EDGE ( 'NONE', *, *, #13888, .F. ) ;
#11252 = CIRCLE ( 'NONE', #9763, 1.500000000000001332 ) ;
#11253 = CARTESIAN_POINT ( 'NONE',  ( -52.26261052913025651, -23.47708768067938578, 8.660254037844417496 ) ) ;
#11254 = ORIENTED_EDGE ( 'NONE', *, *, #5614, .T. ) ;
#11255 = FACE_OUTER_BOUND ( 'NONE', #13242, .T. ) ;
#11256 = CIRCLE ( 'NONE', #1293, 1.500000000000000888 ) ;
#11257 = CARTESIAN_POINT ( 'NONE',  ( -6.326550248787502032E-15, 2.311308694482618949E-14, -130.3485206753969976 ) ) ;
#11258 = DIRECTION ( 'NONE',  ( -0.1566598588826321192, 0.9876526153536342445, 7.798540720466731404E-17 ) ) ;
#11259 = CARTESIAN_POINT ( 'NONE',  ( -81.87192997736543987, 3.395211045985502274, -2.500000000000000000 ) ) ;
#11260 = CARTESIAN_POINT ( 'NONE',  ( 0.000000000000000000, 0.000000000000000000, -35.00000000000000000 ) ) ;
#11261 = CYLINDRICAL_SURFACE ( 'NONE', #363, 1.500000000000000666 ) ;
#11262 = EDGE_LOOP ( 'NONE', ( #3087, #3362, #18056, #8572, #12228, #16902, #5176 ) ) ;
#11263 = FACE_OUTER_BOUND ( 'NONE', #6822, .T. ) ;
#11264 = EDGE_CURVE ( 'NONE', #1614, #482, #12637, .T. ) ;
#11265 = EDGE_CURVE ( 'NONE', #16485, #10686, #2371, .T. ) ;
#11266 = CARTESIAN_POINT ( 'NONE',  ( -76.90911978745816668, -45.00000000000000711, -20.00000000000000000 ) ) ;
#11267 = LINE ( 'NONE', #12872, #16904 ) ;
#11268 = EDGE_LOOP ( 'NONE', ( #13240, #17938 ) ) ;
#11269 = EDGE_LOOP ( 'NONE', ( #14795, #5495 ) ) ;
#11270 = DIRECTION ( 'NONE',  ( -0.9876526153536341335, -0.1566598588826327021, 0.000000000000000000 ) ) ;
#11271 = MECHANICAL_DESIGN_GEOMETRIC_PRESENTATION_REPRESENTATION (  '', ( #18286 ), #10056 ) ;
#11272 = ORIENTED_EDGE ( 'NONE', *, *, #10990, .T. ) ;
#11273 = ORIENTED_EDGE ( 'NONE', *, *, #12839, .T. ) ;
#11274 = ORIENTED_EDGE ( 'NONE', *, *, #15392, .F. ) ;
#11275 = CARTESIAN_POINT ( 'NONE',  ( -61.84966369593023927, -30.06027927571514624, -21.65063509461098334 ) ) ;
#11276 = B_SPLINE_CURVE_WITH_KNOTS ( 'NONE', 3,
 ( #804, #12331, #11104, #13962, #2301, #5154, #12618, #13756, #5254, #3891, #5349, #16929, #9801, #6586, #15568, #18573, #18180, #6692 ),
 .UNSPECIFIED., .F., .F.,
 ( 4, 2, 2, 2, 2, 2, 2, 2, 4 ),
 ( 0.000000000000000000, 0.0006036110467293982285, 0.001207222093458796457, 0.001810833140188194794, 0.002414444186917592914, 0.003018055233646991034, 0.003621666280376389588, 0.004225277327105787274, 0.004828888373835185828 ),
 .UNSPECIFIED. ) ;
#11277 = FACE_BOUND ( 'NONE', #9238, .T. ) ;
#11278 = DIRECTION ( 'NONE',  ( -0.1566598588826321192, 0.9876526153536342445, 7.798540720466730171E-17 ) ) ;
#11279 = AXIS2_PLACEMENT_3D ( 'NONE', #1443, #10231, #3032 ) ;
#11280 = DIRECTION ( 'NONE',  ( -0.1566598588826321192, 0.9876526153536342445, 7.798540720466731404E-17 ) ) ;
#11281 = EDGE_CURVE ( 'NONE', #17456, #15676, #5218, .T. ) ;
#11282 = DIRECTION ( 'NONE',  ( -0.9876526153536336894, -0.1566598588826350336, 0.000000000000000000 ) ) ;
#11283 = DIRECTION ( 'NONE',  ( -0.1566598588826321192, 0.9876526153536342445, 7.798540720466730171E-17 ) ) ;
#11284 = FACE_OUTER_BOUND ( 'NONE', #7854, .T. ) ;
#11285 = DIRECTION ( 'NONE',  ( 0.000000000000000000, 0.000000000000000000, 1.000000000000000000 ) ) ;
#11286 = LINE ( 'NONE', #17105, #5421 ) ;
#11287 = EDGE_CURVE ( 'NONE', #4611, #7789, #16299, .T. ) ;
#11288 = ORIENTED_EDGE ( 'NONE', *, *, #17153, .T. ) ;
#11289 = EDGE_LOOP ( 'NONE', ( #7832, #14430 ) ) ;
#11290 = ORIENTED_EDGE ( 'NONE', *, *, #8262, .T. ) ;
#11291 = FACE_OUTER_BOUND ( 'NONE', #4847, .T. ) ;
#11292 = VECTOR ( 'NONE', #1774, 1000.000000000000000 ) ;
#11293 = VERTEX_POINT ( 'NONE', #16493 ) ;
#11294 = ORIENTED_EDGE ( 'NONE', *, *, #15551, .F. ) ;
#11295 = DIRECTION ( 'NONE',  ( -0.9876526153536341335, -0.1566598588826327021, 0.000000000000000000 ) ) ;
#11296 = CARTESIAN_POINT ( 'NONE',  ( -35.63723437888118184, -83.60797445167352748, 17.32050807568881368 ) ) ;
#11297 = ORIENTED_EDGE ( 'NONE', *, *, #8503, .T. ) ;
#11298 = PRODUCT_DEFINITION_CONTEXT ( 'detailed design', #13654, 'design' ) ;
#11299 = FACE_OUTER_BOUND ( 'NONE', #11401, .T. ) ;
#11300 = APPLICATION_PROTOCOL_DEFINITION ( 'draft international standard', 'automotive_design', 1998, #13654 ) ;
#11301 = CARTESIAN_POINT ( 'NONE',  ( -36.62488699423479943, -83.76463431055617548, 4.330127018922213189 ) ) ;
#11302 = ORIENTED_EDGE ( 'NONE', *, *, #2870, .F. ) ;
#11303 = DIRECTION ( 'NONE',  ( -0.9876526153536341335, -0.1566598588826327021, 0.000000000000000000 ) ) ;
#11304 = DIRECTION ( 'NONE',  ( -0.9876526153536341335, -0.1566598588826327021, 0.000000000000000000 ) ) ;
#11305 = ORIENTED_EDGE ( 'NONE', *, *, #17550, .F. ) ;
#11306 = ORIENTED_EDGE ( 'NONE', *, *, #16111, .F. ) ;
#11307 = DIRECTION ( 'NONE',  ( -0.9876526153536341335, -0.1566598588826327576, 0.000000000000000000 ) ) ;
#11308 = CARTESIAN_POINT ( 'NONE',  ( -17.69476899175320739, -17.99399261978727438, 17.32050807568881012 ) ) ;
#11309 = ORIENTED_EDGE ( 'NONE', *, *, #191, .F. ) ;
#11310 = EDGE_CURVE ( 'NONE', #3748, #11897, #8129, .T. ) ;
#11311 = LINE ( 'NONE', #17130, #2711 ) ;
#11312 = ORIENTED_EDGE ( 'NONE', *, *, #8184, .T. ) ;
#11313 = DIRECTION ( 'NONE',  ( 0.000000000000000000, 0.000000000000000000, -1.000000000000000000 ) ) ;
#11314 = EDGE_CURVE ( 'NONE', #5645, #16215, #18769, .T. ) ;
#11315 = CARTESIAN_POINT ( 'NONE',  ( -89.99999999999998579, -35.00000000000001421, 2.500000000000000000 ) ) ;
#11316 = CARTESIAN_POINT ( 'NONE',  ( -126.9542992265478887, 9.594132765015094932, 2.584671478510879528 ) ) ;
#11317 = DIRECTION ( 'NONE',  ( -1.000000000000000000, 0.000000000000000000, 0.000000000000000000 ) ) ;
#11318 = CARTESIAN_POINT ( 'NONE',  ( -81.73462711737164454, 33.01666666666666572, 35.00000000000000000 ) ) ;
#11319 = DIRECTION ( 'NONE',  ( -0.9876526153536341335, -0.1566598588826327021, 0.000000000000000000 ) ) ;
#11320 = VERTEX_POINT ( 'NONE', #5105 ) ;
#11321 = CARTESIAN_POINT ( 'NONE',  ( -34.15575545585073058, -83.37298466334958391, 1.424741226644455312E-14 ) ) ;
#11322 = ORIENTED_EDGE ( 'NONE', *, *, #10082, .T. ) ;
#11323 = CARTESIAN_POINT ( 'NONE',  ( -40.61513246582718750, -26.69209230973856251, -21.65063509461098334 ) ) ;
#11324 = DIRECTION ( 'NONE',  ( 0.000000000000000000, 0.000000000000000000, 1.000000000000000000 ) ) ;
#11325 = DIRECTION ( 'NONE',  ( -0.1566598588826321192, 0.9876526153536342445, 7.798540720466731404E-17 ) ) ;
#11326 = VERTEX_POINT ( 'NONE', #7691 ) ;
#11327 = CARTESIAN_POINT ( 'NONE',  ( -81.87959193097326249, 30.50711626588064007, 35.00001199999999102 ) ) ;
#11329 = ORIENTED_EDGE ( 'NONE', *, *, #15337, .F. ) ;
#11328 = CARTESIAN_POINT ( 'NONE',  ( -48.97054468615517919, -85.72288254658906226, 17.32050807568881368 ) ) ;
#11330 = ADVANCED_FACE ( 'NONE', ( #13439 ), #2082, .T. ) ;
#11331 = EDGE_CURVE ( 'NONE', #15461, #11513, #18463, .T. ) ;
#11332 = DIRECTION ( 'NONE',  ( -0.1566598588826321747, 0.9876526153536343555, 0.000000000000000000 ) ) ;
#11333 = CIRCLE ( 'NONE', #14988, 1.500000000000000444 ) ;
#11334 = DIRECTION ( 'NONE',  ( -0.000000000000000000, -0.000000000000000000, -1.000000000000000000 ) ) ;
#11335 = EDGE_LOOP ( 'NONE', ( #12797, #4008 ) ) ;
#11336 = ORIENTED_EDGE ( 'NONE', *, *, #6440, .T. ) ;
#11337 = EDGE_CURVE ( 'NONE', #1532, #16572, #7870, .T. ) ;
#11338 = VERTEX_POINT ( 'NONE', #6272 ) ;
#11339 = CARTESIAN_POINT ( 'NONE',  ( -62.30385499342917655, -87.83779064150458282, 8.660254037844412167 ) ) ;
#11340 = ORIENTED_EDGE ( 'NONE', *, *, #16432, .T. ) ;
#11341 = LINE ( 'NONE', #17159, #11222 ) ;
#11342 = LINE ( 'NONE', #14312, #4929 ) ;
#11343 = DIRECTION ( 'NONE',  ( 0.000000000000000000, 0.000000000000000000, 1.000000000000000000 ) ) ;
#11344 = CARTESIAN_POINT ( 'NONE',  ( -6.995308533625909320, -79.06483854407721878, -4.330127018922185655 ) ) ;
#11345 = CARTESIAN_POINT ( 'NONE',  ( -30.53425299135042081, -20.03057078526147805, -8.660254037844380193 ) ) ;
#11346 = DIRECTION ( 'NONE',  ( -0.9876526153536336894, -0.1566598588826349503, 0.000000000000000000 ) ) ;
#11347 = CIRCLE ( 'NONE', #6543, 1.500000000000000888 ) ;
#11348 = CARTESIAN_POINT ( 'NONE',  ( -14.44233815895597672, -22.54060604934882051, 4.330127018922217630 ) ) ;
#11349 = B_SPLINE_CURVE_WITH_KNOTS ( 'NONE', 3,
 ( #11259, #5400, #2260, #18133, #2465, #18244 ),
 .UNSPECIFIED., .F., .F.,
 ( 4, 2, 4 ),
 ( 3.705370968959021185E-18, 0.001760439274641287504, 0.003520878549282571539 ),
 .UNSPECIFIED. ) ;
#11350 = DIRECTION ( 'NONE',  ( -0.9876526153536336894, -0.1566598588826349503, 0.000000000000000000 ) ) ;
#11351 = EDGE_LOOP ( 'NONE', ( #10571, #2920, #4237, #18064 ) ) ;
#11352 = EDGE_CURVE ( 'NONE', #17569, #8605, #4479, .T. ) ;
#11354 = ORIENTED_EDGE ( 'NONE', *, *, #5902, .F. ) ;
#11353 = EDGE_CURVE ( 'NONE', #9249, #10116, #3392, .T. ) ;
#11355 = APPLICATION_CONTEXT ( 'automotive_design' ) ;
#11356 = LINE ( 'NONE', #17177, #8456 ) ;
#11357 = PRODUCT_DEFINITION_SHAPE ( 'NONE', 'NONE',  #18802 ) ;
#11358 = ORIENTED_EDGE ( 'NONE', *, *, #14049, .T. ) ;
#11359 = ORIENTED_EDGE ( 'NONE', *, *, #7293, .F. ) ;
#11360 = ORIENTED_EDGE ( 'NONE', *, *, #9298, .T. ) ;
#11361 = DIRECTION ( 'NONE',  ( -0.1566598588826321192, 0.9876526153536342445, 7.798540720466730171E-17 ) ) ;
#11362 = VECTOR ( 'NONE', #4529, 1000.000000000000000 ) ;
#11363 = PRODUCT_DEFINITION ( 'UNKNOWN', '', #15965, #7769 ) ;
#11364 = CYLINDRICAL_SURFACE ( 'NONE', #12453, 1.500000000000001554 ) ;
#11365 = EDGE_CURVE ( 'NONE', #17063, #4741, #1986, .T. ) ;
#11366 = CARTESIAN_POINT ( 'NONE',  ( 0.000000000000000000, 0.000000000000000000, 24.99999999999999289 ) ) ;
#11367 = ORIENTED_EDGE ( 'NONE', *, *, #10860, .F. ) ;
#11368 = FACE_BOUND ( 'NONE', #10704, .T. ) ;
#11369 = EDGE_LOOP ( 'NONE', ( #16647, #2542, #3607, #8904, #9292, #13323, #4806 ) ) ;
#11370 = CARTESIAN_POINT ( 'NONE',  ( -19.87442754340095519, -23.40223527320329922, 8.660254037844417496 ) ) ;
#11371 = CARTESIAN_POINT ( 'NONE',  ( 55.85952145814821534, 6.938893903907228378E-15, -35.00000000000000000 ) ) ;
#11372 = CIRCLE ( 'NONE', #2010, 1.500000000000001332 ) ;
#11373 = CARTESIAN_POINT ( 'NONE',  ( -34.15575545585073058, -83.37298466334958391, 17.32050807568881368 ) ) ;
#11374 = DIRECTION ( 'NONE',  ( -0.9876526153536344665, -0.1566598588826304539, 0.000000000000000000 ) ) ;
#11375 = ORIENTED_EDGE ( 'NONE', *, *, #18358, .T. ) ;
#11376 = CYLINDRICAL_SURFACE ( 'NONE', #6634, 1.500000000000001554 ) ;
#11377 = VERTEX_POINT ( 'NONE', #677 ) ;
#11378 = ORIENTED_EDGE ( 'NONE', *, *, #4042, .F. ) ;
#11379 = VERTEX_POINT ( 'NONE', #15163 ) ;
#11380 = DIRECTION ( 'NONE',  ( -0.1566598588826321192, 0.9876526153536342445, 7.798540720466730171E-17 ) ) ;
#11381 = VECTOR ( 'NONE', #13159, 1000.000000000000114 ) ;
#11382 = ORIENTED_EDGE ( 'NONE', *, *, #6193, .T. ) ;
#11383 = FACE_OUTER_BOUND ( 'NONE', #6826, .T. ) ;
#11384 = EDGE_CURVE ( 'NONE', #17992, #983, #2060, .T. ) ;
#11385 = CARTESIAN_POINT ( 'NONE',  ( -44.56574292724170760, -27.31873174526908699, 17.32050807568881723 ) ) ;
#11386 = ADVANCED_FACE ( 'NONE', ( #17950 ), #6934, .T. ) ;
#11387 = STYLED_ITEM ( 'NONE', ( #3163 ), #14964 ) ;
#11388 = PLANE ( 'NONE',  #2774 ) ;
#11389 = EDGE_CURVE ( 'NONE', #14949, #8287, #1182, .T. ) ;
#11390 = CIRCLE ( 'NONE', #4447, 1.500000000000000444 ) ;
#11391 = DIRECTION ( 'NONE',  ( 0.000000000000000000, 0.000000000000000000, 1.000000000000000000 ) ) ;
#11392 = CARTESIAN_POINT ( 'NONE',  ( -41.56315007100294423, -84.54793360496931598, 12.99038105676661203 ) ) ;
#11393 = CYLINDRICAL_SURFACE ( 'NONE', #11772, 1.500000000000001554 ) ;
#11394 = ORIENTED_EDGE ( 'NONE', *, *, #17782, .F. ) ;
#11395 = DIRECTION ( 'NONE',  ( -0.9876526153536341335, -0.1566598588826327021, 0.000000000000000000 ) ) ;
#11396 = CARTESIAN_POINT ( 'NONE',  ( -20.16390053013728334, -18.38564226699384463, -21.65063509461098334 ) ) ;
#11397 = LINE ( 'NONE', #10358, #6847 ) ;
#11398 = ORIENTED_EDGE ( 'NONE', *, *, #14498, .F. ) ;
#11399 = VERTEX_POINT ( 'NONE', #10774 ) ;
#11400 = DIRECTION ( 'NONE',  ( -0.1566598588826321192, 0.9876526153536342445, 7.798540720466730171E-17 ) ) ;
#11401 = EDGE_LOOP ( 'NONE', ( #12210, #16538, #11745, #14774 ) ) ;
#11402 = MECHANICAL_DESIGN_GEOMETRIC_PRESENTATION_REPRESENTATION (  '', ( #10198 ), #16579 ) ;
#11403 = AXIS2_PLACEMENT_3D ( 'NONE', #13622, #12388, #16577 ) ;
#11404 = DIRECTION ( 'NONE',  ( -0.1566598588826321747, 0.9876526153536343555, 0.000000000000000000 ) ) ;
#11405 = EDGE_LOOP ( 'NONE', ( #7344, #10189 ) ) ;
#11406 = CARTESIAN_POINT ( 'NONE',  ( -0.4108482230646692823, -15.25244508934120802, -4.330127018922183879 ) ) ;
#11407 = CARTESIAN_POINT ( 'NONE',  ( -51.43967622453926936, -86.11453219379563961, -4.330127018922185655 ) ) ;
#11408 = CARTESIAN_POINT ( 'NONE',  ( -70.00000000000000000, 44.99999999999999289, 2.500000000000000000 ) ) ;
#11409 = ADVANCED_FACE ( 'NONE', ( #16590 ), #7959, .F. ) ;
#11410 = CYLINDRICAL_SURFACE ( 'NONE', #2356, 1.500000000000001554 ) ;
#11411 = SURFACE_STYLE_USAGE ( .BOTH. , #18689 ) ;
#11412 = AXIS2_PLACEMENT_3D ( 'NONE', #3072, #8865, #14646 ) ;
#11413 = DIRECTION ( 'NONE',  ( 0.000000000000000000, 0.000000000000000000, 1.000000000000000000 ) ) ;
#11414 = ORIENTED_EDGE ( 'NONE', *, *, #18466, .T. ) ;
#11415 = DIRECTION ( 'NONE',  ( -2.735665993912342121E-16, -0.000000000000000000, -1.000000000000000000 ) ) ;
#11416 = ADVANCED_FACE ( 'NONE', ( #9770 ), #12868, .F. ) ;
#11417 = CARTESIAN_POINT ( 'NONE',  ( -33.99103714508810725, -20.57888029135069274, 1.908195823574487804E-14 ) ) ;
#11418 = FACE_OUTER_BOUND ( 'NONE', #5579, .T. ) ;
#11419 = ORIENTED_EDGE ( 'NONE', *, *, #11094, .T. ) ;
#11420 = DIRECTION ( 'NONE',  ( -0.1566598588826321192, 0.9876526153536342445, 7.798540720466730171E-17 ) ) ;
#11421 = AXIS2_PLACEMENT_3D ( 'NONE', #6351, #9358, #3463 ) ;
#11422 = EDGE_CURVE ( 'NONE', #14703, #8123, #8450, .T. ) ;
#11423 = LINE ( 'NONE', #6920, #13834 ) ;
#11425 = ORIENTED_EDGE ( 'NONE', *, *, #6164, .T. ) ;
#11424 = DIRECTION ( 'NONE',  ( -0.1566598588826321192, 0.9876526153536342445, 7.798540720466730171E-17 ) ) ;
#11426 = AXIS2_PLACEMENT_3D ( 'NONE', #13863, #12531, #8000 ) ;
#11427 = FACE_OUTER_BOUND ( 'NONE', #10102, .T. ) ;
#11428 = ORIENTED_EDGE ( 'NONE', *, *, #727, .T. ) ;
#11429 = DIRECTION ( 'NONE',  ( -0.1566598588826321747, 0.9876526153536343555, 0.000000000000000000 ) ) ;
#11430 = DIRECTION ( 'NONE',  ( -0.1566598588826321192, 0.9876526153536342445, 7.798540720466730171E-17 ) ) ;
#11431 = CARTESIAN_POINT ( 'NONE',  ( -24.31886431249228053, -24.10720463817513703, -21.65063509461098334 ) ) ;
#11432 = AXIS2_PLACEMENT_3D ( 'NONE', #12434, #6864, #10998 ) ;
#11433 = LINE ( 'NONE', #4427, #3088 ) ;
#11434 = CARTESIAN_POINT ( 'NONE',  ( -76.95392591297100182, -27.39358415274517711, 8.660254037844417496 ) ) ;
#11435 = AXIS2_PLACEMENT_3D ( 'NONE', #6180, #10511, #5546 ) ;
#11436 = ADVANCED_FACE ( 'NONE', ( #14109 ), #4049, .F. ) ;
#11437 = CARTESIAN_POINT ( 'NONE',  ( -12.75650591498505371, -17.21069332537411256, -8.660254037844380193 ) ) ;
#11438 = CIRCLE ( 'NONE', #12032, 2.500000000000002220 ) ;
#11439 = DIRECTION ( 'NONE',  ( -0.000000000000000000, -0.000000000000000000, -1.000000000000000000 ) ) ;
#11440 = AXIS2_PLACEMENT_3D ( 'NONE', #5688, #16104, #4252 ) ;
#11441 = ADVANCED_FACE ( 'NONE', ( #1341 ), #12672, .F. ) ;
#11442 = DIRECTION ( 'NONE',  ( 3.816390434826605238E-17, 0.000000000000000000, -1.000000000000000000 ) ) ;
#11443 = VERTEX_POINT ( 'NONE', #6835 ) ;
#11444 = ORIENTED_EDGE ( 'NONE', *, *, #8015, .F. ) ;
#11445 = CARTESIAN_POINT ( 'NONE',  ( -45.55339554259532520, -27.47539160415171722, 12.99038105676661736 ) ) ;
#11446 = CIRCLE ( 'NONE', #13876, 1.499999999999999556 ) ;
#11447 = ORIENTED_EDGE ( 'NONE', *, *, #669, .F. ) ;
#11448 = ORIENTED_EDGE ( 'NONE', *, *, #18162, .F. ) ;
#11449 = DIRECTION ( 'NONE',  ( -0.9876526153536341335, -0.1566598588826327021, 0.000000000000000000 ) ) ;
#11450 = CIRCLE ( 'NONE', #15403, 15.83618137761393463 ) ;
#11451 = ORIENTED_EDGE ( 'NONE', *, *, #4367, .F. ) ;
#11452 = CIRCLE ( 'NONE', #15718, 1.500000000000000000 ) ;
#11453 = FACE_BOUND ( 'NONE', #16593, .T. ) ;
#11454 = ORIENTED_EDGE ( 'NONE', *, *, #9898, .F. ) ;
#11455 = ADVANCED_FACE ( 'NONE', ( #14210 ), #18533, .F. ) ;
#11456 = VECTOR ( 'NONE', #14097, 1000.000000000000000 ) ;
#11457 = EDGE_CURVE ( 'NONE', #13719, #2279, #17838, .T. ) ;
#11458 = CIRCLE ( 'NONE', #7268, 12.74754878398196567 ) ;
#11459 = ORIENTED_EDGE ( 'NONE', *, *, #15667, .T. ) ;
#11460 = AXIS2_PLACEMENT_3D ( 'NONE', #5857, #2817, #14380 ) ;
#11461 = VERTEX_POINT ( 'NONE', #17275 ) ;
#11462 = DIRECTION ( 'NONE',  ( -0.9876526153536336894, -0.1566598588826349503, 0.000000000000000000 ) ) ;
#11463 = CIRCLE ( 'NONE', #1216, 1.500000000000000888 ) ;
#11464 = VECTOR ( 'NONE', #8808, 1000.000000000000000 ) ;
#11465 = AXIS2_PLACEMENT_3D ( 'NONE', #11774, #2813, #16171 ) ;
#11466 = CARTESIAN_POINT ( 'NONE',  ( -20.86208015875458344, -23.55889513208593655, -4.330127018922181215 ) ) ;
#11467 = CARTESIAN_POINT ( 'NONE',  ( 55.85952145814821534, 6.938893903907228378E-15, -35.00000000000000000 ) ) ;
#11468 = DIRECTION ( 'NONE',  ( -0.1566598588826321192, 0.9876526153536342445, 7.798540720466731404E-17 ) ) ;
#11469 = ORIENTED_EDGE ( 'NONE', *, *, #4293, .F. ) ;
#11470 = VERTEX_POINT ( 'NONE', #7039 ) ;
#11471 = AXIS2_PLACEMENT_3D ( 'NONE', #2146, #6712, #14282 ) ;
#11472 = VERTEX_POINT ( 'NONE', #2357 ) ;
#11473 = CARTESIAN_POINT ( 'NONE',  ( 0.000000000000000000, 0.000000000000000000, 35.00000000000000000 ) ) ;
#11474 = CIRCLE ( 'NONE', #6044, 1.500000000000000000 ) ;
#11475 = ORIENTED_EDGE ( 'NONE', *, *, #5692, .T. ) ;
#11476 = VECTOR ( 'NONE', #18166, 1000.000000000000000 ) ;
#11477 = DIRECTION ( 'NONE',  ( -1.000000000000000000, -0.000000000000000000, -0.000000000000000000 ) ) ;
#11478 = CARTESIAN_POINT ( 'NONE',  ( -65.30644784966793281, -30.60858878180435738, -21.65063509461098334 ) ) ;
#11479 = AXIS2_PLACEMENT_3D ( 'NONE', #17337, #14081, #10095 ) ;
#11480 = DIRECTION ( 'NONE',  ( -0.1566598588826321192, 0.9876526153536342445, 7.798540720466730171E-17 ) ) ;
#11481 = CARTESIAN_POINT ( 'NONE',  ( -9.504075082187826595, -21.75730675493566579, -21.65063509461098334 ) ) ;
#11482 = SHAPE_DEFINITION_REPRESENTATION ( #11041, #6739 ) ;
#11483 = VECTOR ( 'NONE', #15674, 1000.000000000000114 ) ;
#11484 = CARTESIAN_POINT ( 'NONE',  ( -174.8836385705398300, 55.21907105134628324, 5.316095106350546828 ) ) ;
#11486 = FACE_OUTER_BOUND ( 'NONE', #11369, .T. ) ;
#11485 = CIRCLE ( 'NONE', #8186, 1.500000000000001332 ) ;
#11487 = EDGE_CURVE ( 'NONE', #2990, #8008, #9650, .T. ) ;
#11488 = DIRECTION ( 'NONE',  ( 1.438274729681541621E-16, 6.252920376642371210E-17, -1.000000000000000000 ) ) ;
#11489 = CIRCLE ( 'NONE', #9716, 3.000000000000000000 ) ;
#11490 = ORIENTED_EDGE ( 'NONE', *, *, #15768, .T. ) ;
#11491 = EDGE_CURVE ( 'NONE', #14533, #9448, #13557, .T. ) ;
#11492 = ORIENTED_EDGE ( 'NONE', *, *, #1080, .F. ) ;
#11493 = FACE_OUTER_BOUND ( 'NONE', #9247, .T. ) ;
#11494 = ORIENTED_EDGE ( 'NONE', *, *, #17129, .T. ) ;
#11495 = VECTOR ( 'NONE', #2077, 1000.000000000000000 ) ;
#11496 = DIRECTION ( 'NONE',  ( -0.1566598588826321192, 0.9876526153536342445, 7.798540720466731404E-17 ) ) ;
#11497 = DIRECTION ( 'NONE',  ( -0.1566598588826321192, 0.9876526153536342445, 7.798540720466730171E-17 ) ) ;
#11498 = ORIENTED_EDGE ( 'NONE', *, *, #16016, .F. ) ;
#11499 = VERTEX_POINT ( 'NONE', #11345 ) ;
#11500 = DIRECTION ( 'NONE',  ( 0.000000000000000000, 0.000000000000000000, 1.000000000000000000 ) ) ;
#11501 = CIRCLE ( 'NONE', #3327, 1.499999999999999556 ) ;
#11502 = CIRCLE ( 'NONE', #12724, 1.500000000000000444 ) ;
#11503 = CARTESIAN_POINT ( 'NONE',  ( -11.97320662057189899, -22.14895640214223960, -17.32050807568878170 ) ) ;
#11504 = CARTESIAN_POINT ( 'NONE',  ( -128.7754985213482257, 9.229958444745710366, 4.052748550462855093 ) ) ;
#11505 = CARTESIAN_POINT ( 'NONE',  ( 3.000000000000000000, 3.673940397442059868E-16, -35.00000000000000000 ) ) ;
#11506 = CARTESIAN_POINT ( 'NONE',  ( -75.96627329761737712, -27.23692429386253622, -4.330127018922180326 ) ) ;
#11507 = CIRCLE ( 'NONE', #14560, 1.500000000000001332 ) ;
#11508 = CARTESIAN_POINT ( 'NONE',  ( -51.47931123471711601, -28.41535075744751282, -17.32050807568878170 ) ) ;
#11509 = CARTESIAN_POINT ( 'NONE',  ( -29.21749237908259644, -82.58968536893641499, -17.32050807568878525 ) ) ;
#11510 = VECTOR ( 'NONE', #11886, 1000.000000000000000 ) ;
#11511 = LINE ( 'NONE', #14840, #7433 ) ;
#11512 = CARTESIAN_POINT ( 'NONE',  ( -46.33669483700848701, -22.53712852738358663, -4.330127018922180326 ) ) ;
#11513 = VERTEX_POINT ( 'NONE', #7123 ) ;
#11514 = DIRECTION ( 'NONE',  ( -0.1566598588826321192, 0.9876526153536342445, 7.798540720466730171E-17 ) ) ;
#11515 = AXIS2_PLACEMENT_3D ( 'NONE', #3814, #926, #8208 ) ;
#11517 = ORIENTED_EDGE ( 'NONE', *, *, #16634, .F. ) ;
#11516 = DIRECTION ( 'NONE',  ( -0.1566598588826321192, 0.9876526153536342445, 7.798540720466730171E-17 ) ) ;
#11518 = CIRCLE ( 'NONE', #7327, 1.500000000000000888 ) ;
#11519 = EDGE_CURVE ( 'NONE', #16333, #411, #4255, .T. ) ;
#11520 = DIRECTION ( 'NONE',  ( -0.1566598588826321192, 0.9876526153536342445, 7.798540720466730171E-17 ) ) ;
#11521 = ORIENTED_EDGE ( 'NONE', *, *, #4516, .T. ) ;
#11522 = VECTOR ( 'NONE', #16834, 1000.000000000000000 ) ;
#11523 = DIRECTION ( 'NONE',  ( -0.1566598588826321192, 0.9876526153536342445, 7.798540720466730171E-17 ) ) ;
#11524 = EDGE_CURVE ( 'NONE', #11126, #8986, #5505, .T. ) ;
#11525 = AXIS2_PLACEMENT_3D ( 'NONE', #17439, #2546, #8529 ) ;
#11526 = CIRCLE ( 'NONE', #6424, 1.500000000000001332 ) ;
#11527 = CARTESIAN_POINT ( 'NONE',  ( -77.44775222064782838, -27.47191408218649045, 12.99038105676661736 ) ) ;
#11528 = DIRECTION ( 'NONE',  ( -0.1566598588826321192, 0.9876526153536342445, 7.798540720466730171E-17 ) ) ;
#11529 = ORIENTED_EDGE ( 'NONE', *, *, #5114, .F. ) ;
#11530 = DIRECTION ( 'NONE',  ( -0.000000000000000000, -0.000000000000000000, -1.000000000000000000 ) ) ;
#11531 = FACE_OUTER_BOUND ( 'NONE', #10441, .T. ) ;
#11532 = CIRCLE ( 'NONE', #2779, 2.199999999999993516 ) ;
#11533 = CARTESIAN_POINT ( 'NONE',  ( -50.49165861936349131, -28.25869089856488614, -12.99038105676658006 ) ) ;
#11534 = DIRECTION ( 'NONE',  ( -0.9876526153536336894, -0.1566598588826349503, 0.000000000000000000 ) ) ;
#11535 = FACE_BOUND ( 'NONE', #13534, .T. ) ;
#11536 = FACE_OUTER_BOUND ( 'NONE', #18745, .T. ) ;
#11537 = ORIENTED_EDGE ( 'NONE', *, *, #1877, .F. ) ;
#11538 = CIRCLE ( 'NONE', #13976, 150.0000000000000284 ) ;
#11539 = ORIENTED_EDGE ( 'NONE', *, *, #5862, .T. ) ;
#11540 = DIRECTION ( 'NONE',  ( -0.1566598588826321747, 0.9876526153536343555, 0.000000000000000000 ) ) ;
#11541 = EDGE_CURVE ( 'NONE', #16711, #10603, #12354, .T. ) ;
#11542 = EDGE_LOOP ( 'NONE', ( #7488, #15805, #8802, #15052 ) ) ;
#11543 = VERTEX_POINT ( 'NONE', #11437 ) ;
#11544 = ORIENTED_EDGE ( 'NONE', *, *, #14376, .T. ) ;
#11545 = CARTESIAN_POINT ( 'NONE',  ( -41.39843176024032800, -21.75382923297043547, 12.99038105676661736 ) ) ;
#11546 = VECTOR ( 'NONE', #18105, 1000.000000000000000 ) ;
#11547 = ORIENTED_EDGE ( 'NONE', *, *, #11264, .F. ) ;
#11548 = ORIENTED_EDGE ( 'NONE', *, *, #12756, .F. ) ;
#11549 = FACE_BOUND ( 'NONE', #9113, .T. ) ;
#11550 = ADVANCED_FACE ( 'NONE', ( #17080 ), #8149, .F. ) ;
#11551 = CARTESIAN_POINT ( 'NONE',  ( -57.85941822433786541, -87.13282127653273790, -4.330127018922185655 ) ) ;
#11552 = CARTESIAN_POINT ( 'NONE',  ( -29.05277406831996245, -19.79558099693753093, -8.660254037844380193 ) ) ;
#11553 = ORIENTED_EDGE ( 'NONE', *, *, #10577, .F. ) ;
#11554 = CIRCLE ( 'NONE', #13990, 1.499999999999999556 ) ;
#11555 = FACE_OUTER_BOUND ( 'NONE', #13946, .T. ) ;
#11556 = ORIENTED_EDGE ( 'NONE', *, *, #11791, .T. ) ;
#11557 = FACE_BOUND ( 'NONE', #8597, .T. ) ;
#11558 = CARTESIAN_POINT ( 'NONE',  ( 0.000000000000000000, 0.000000000000000000, -30.00000000000000000 ) ) ;
#11559 = AXIS2_PLACEMENT_3D ( 'NONE', #5890, #5710, #4547 ) ;
#11560 = DIRECTION ( 'NONE',  ( -0.9876526153536336894, -0.1566598588826349503, 0.000000000000000000 ) ) ;
#11561 = VECTOR ( 'NONE', #13754, 1000.000000000000000 ) ;
#11562 = CARTESIAN_POINT ( 'NONE',  ( 2.881217619910392269, -77.49823995525089515, -12.99038105676658539 ) ) ;
#11563 = CARTESIAN_POINT ( 'NONE',  ( 3.267113004676621661E-15, 1.140077944303684267E-15, -20.00000000000000355 ) ) ;
#11564 = FACE_BOUND ( 'NONE', #9009, .T. ) ;
#11565 = DIRECTION ( 'NONE',  ( 0.000000000000000000, 0.000000000000000000, 1.000000000000000000 ) ) ;
#11566 = DIRECTION ( 'NONE',  ( -1.000000000000000000, 0.000000000000000000, 0.000000000000000000 ) ) ;
#11567 = EDGE_LOOP ( 'NONE', ( #1794, #2792 ) ) ;
#11568 = EDGE_LOOP ( 'NONE', ( #11606, #15329, #11290, #7253 ) ) ;
#11569 = ORIENTED_EDGE ( 'NONE', *, *, #7054, .F. ) ;
#11570 = DIRECTION ( 'NONE',  ( -0.1566598588826321192, 0.9876526153536342445, 7.798540720466730171E-17 ) ) ;
#11571 = EDGE_CURVE ( 'NONE', #10712, #11171, #1488, .T. ) ;
#11572 = EDGE_CURVE ( 'NONE', #17136, #6756, #7537, .T. ) ;
#11573 = ORIENTED_EDGE ( 'NONE', *, *, #14660, .T. ) ;
#11574 = CARTESIAN_POINT ( 'NONE',  ( -61.84966369593024638, -30.06027927571514624, -4.330127018922181215 ) ) ;
#11575 = EDGE_CURVE ( 'NONE', #17944, #10450, #12578, .T. ) ;
#11576 = DIRECTION ( 'NONE',  ( -0.9876526153536341335, -0.1566598588826327021, 0.000000000000000000 ) ) ;
#11577 = CIRCLE ( 'NONE', #8276, 1.499999999999999556 ) ;
#11578 = EDGE_CURVE ( 'NONE', #17378, #4142, #175, .T. ) ;
#11579 = EDGE_CURVE ( 'NONE', #518, #7954, #3868, .T. ) ;
#11580 = CARTESIAN_POINT ( 'NONE',  ( -49.95819730150881099, -85.87954240547168183, -4.330127018922185655 ) ) ;
#11581 = CARTESIAN_POINT ( 'NONE',  ( -3.044698072211382112, -78.43819910854666944, -8.660254037844385522 ) ) ;
#11582 = SHAPE_DEFINITION_REPRESENTATION ( #16837, #13127 ) ;
#11583 = VERTEX_POINT ( 'NONE', #7216 ) ;
#11584 = CARTESIAN_POINT ( 'NONE',  ( -174.8436531212914815, 55.46571492669004755, 4.766626691765358359 ) ) ;
#11585 = CARTESIAN_POINT ( 'NONE',  ( -48.80582637539257718, -22.92877817459016043, -17.32050807568878170 ) ) ;
#11586 = CARTESIAN_POINT ( 'NONE',  ( -36.46016868347218320, -20.97052993855727721, 12.99038105676661736 ) ) ;
#11587 = B_SPLINE_CURVE_WITH_KNOTS ( 'NONE', 3,
 ( #16888, #15246, #11160, #14105 ),
 .UNSPECIFIED., .F., .F.,
 ( 4, 4 ),
 ( 0.000000000000000000, 0.003000475340473835600 ),
 .UNSPECIFIED. ) ;
#11588 = VERTEX_POINT ( 'NONE', #11889 ) ;
#11589 = ORIENTED_EDGE ( 'NONE', *, *, #2111, .T. ) ;
#11590 = LINE ( 'NONE', #15964, #17232 ) ;
#11591 = DIRECTION ( 'NONE',  ( -0.1566598588826321192, 0.9876526153536342445, 7.798540720466730171E-17 ) ) ;
#11592 = LINE ( 'NONE', #7364, #10186 ) ;
#11593 = EDGE_CURVE ( 'NONE', #18515, #1621, #14489, .T. ) ;
#11594 = LINE ( 'NONE', #14917, #14814 ) ;
#11595 = ORIENTED_EDGE ( 'NONE', *, *, #12887, .F. ) ;
#11596 = CARTESIAN_POINT ( 'NONE',  ( -20.16390053013728689, -18.38564226699385173, -4.330127018922180326 ) ) ;
#11597 = VERTEX_POINT ( 'NONE', #15830 ) ;
#11598 = EDGE_CURVE ( 'NONE', #12109, #11293, #5099, .T. ) ;
#11599 = EDGE_CURVE ( 'NONE', #8740, #10626, #4619, .T. ) ;
#11600 = CARTESIAN_POINT ( 'NONE',  ( -39.62747985047356281, -26.53543245085591806, 17.32050807568881723 ) ) ;
#11601 = CARTESIAN_POINT ( 'NONE',  ( -16.70711637639958269, -17.83733276090463704, 4.330127018922218518 ) ) ;
#11602 = APPLICATION_PROTOCOL_DEFINITION ( 'draft international standard', 'automotive_design', 1998, #18202 ) ;
#11603 = DIRECTION ( 'NONE',  ( -0.9876526153536341335, -0.1566598588826327021, 0.000000000000000000 ) ) ;
#11604 = CARTESIAN_POINT ( 'NONE',  ( 55.85952145814821534, 6.938893903907228378E-15, 29.99999999999998579 ) ) ;
#11605 = CARTESIAN_POINT ( 'NONE',  ( -15.71946376104596155, -17.68067290202199970, -17.32050807568878170 ) ) ;
#11606 = ORIENTED_EDGE ( 'NONE', *, *, #8041, .F. ) ;
#11607 = CARTESIAN_POINT ( 'NONE',  ( -30.69897130211303349, -82.82467515726037277, -8.660254037844385522 ) ) ;
#11609 = VERTEX_POINT ( 'NONE', #4349 ) ;
#11608 = DIRECTION ( 'NONE',  ( 0.000000000000000000, 0.000000000000000000, 1.000000000000000000 ) ) ;
#11610 = CARTESIAN_POINT ( 'NONE',  ( -10.78120068427780964, -16.89737360760884144, 8.660254037844413944 ) ) ;
#11611 = ORIENTED_EDGE ( 'NONE', *, *, #1147, .T. ) ;
#11612 = CARTESIAN_POINT ( 'NONE',  ( -17.40529600501688279, -23.01058562599671831, -4.330127018922181215 ) ) ;
#11613 = EDGE_CURVE ( 'NONE', #1459, #14963, #12958, .T. ) ;
#11614 = DIRECTION ( 'NONE',  ( -0.1566598588826321747, 0.9876526153536343555, 0.000000000000000000 ) ) ;
#11615 = EDGE_CURVE ( 'NONE', #12140, #9117, #17547, .T. ) ;
#11616 = LINE ( 'NONE', #5871, #10690 ) ;
#11617 = CYLINDRICAL_SURFACE ( 'NONE', #16411, 1.500000000000000666 ) ;
#11618 = DIRECTION ( 'NONE',  ( -0.000000000000000000, -0.000000000000000000, -1.000000000000000000 ) ) ;
#11619 = EDGE_CURVE ( 'NONE', #12390, #8349, #7571, .T. ) ;
#11620 = DIRECTION ( 'NONE',  ( -0.1566598588826321192, 0.9876526153536342445, 7.798540720466731404E-17 ) ) ;
#11621 = VERTEX_POINT ( 'NONE', #8895 ) ;
#11622 = FACE_OUTER_BOUND ( 'NONE', #14078, .T. ) ;
#11623 = DIRECTION ( 'NONE',  ( -0.1566598588826321192, 0.9876526153536342445, 7.798540720466730171E-17 ) ) ;
#11624 = CARTESIAN_POINT ( 'NONE',  ( 0.000000000000000000, 0.000000000000000000, 35.00000000000000000 ) ) ;
#11625 = CIRCLE ( 'NONE', #3451, 1.500000000000000888 ) ;
#11626 = EDGE_LOOP ( 'NONE', ( #15379, #11054, #11079, #2349 ) ) ;
#11627 = ORIENTED_EDGE ( 'NONE', *, *, #6269, .F. ) ;
#11628 = DIRECTION ( 'NONE',  ( 0.000000000000000000, 0.000000000000000000, -1.000000000000000000 ) ) ;
#11629 = ORIENTED_EDGE ( 'NONE', *, *, #4622, .T. ) ;
#11630 = ORIENTED_EDGE ( 'NONE', *, *, #9854, .T. ) ;
#11631 = DIRECTION ( 'NONE',  ( -0.1566598588826321192, 0.9876526153536342445, 7.798540720466730171E-17 ) ) ;
#11632 = EDGE_LOOP ( 'NONE', ( #8840, #17987, #15438, #9577 ) ) ;
#11633 = FACE_BOUND ( 'NONE', #2506, .T. ) ;
#11634 = CARTESIAN_POINT ( 'NONE',  ( -2.057045456857756971, -78.28153924966404986, 12.99038105676660848 ) ) ;
#11635 = ORIENTED_EDGE ( 'NONE', *, *, #358, .F. ) ;
#11636 = EDGE_CURVE ( 'NONE', #1132, #10626, #11450, .T. ) ;
#11637 = EDGE_LOOP ( 'NONE', ( #18024, #6426 ) ) ;
#11638 = FILL_AREA_STYLE ('',( #14787 ) ) ;
#11639 = ORIENTED_EDGE ( 'NONE', *, *, #16137, .F. ) ;
#11640 = DIRECTION ( 'NONE',  ( -0.9876526153536336894, -0.1566598588826349503, 0.000000000000000000 ) ) ;
#11641 = DIRECTION ( 'NONE',  ( -0.9876526153536336894, -0.1566598588826350336, 0.000000000000000000 ) ) ;
#11643 = ADVANCED_FACE ( 'NONE', ( #5876 ), #16107, .F. ) ;
#11642 = FACE_OUTER_BOUND ( 'NONE', #156, .T. ) ;
#11644 = DIRECTION ( 'NONE',  ( -0.1566598588826321747, 0.9876526153536343555, 0.000000000000000000 ) ) ;
#11645 = AXIS2_PLACEMENT_3D ( 'NONE', #3704, #18363, #1002 ) ;
#11646 = ORIENTED_EDGE ( 'NONE', *, *, #16207, .T. ) ;
#11647 = VERTEX_POINT ( 'NONE', #10393 ) ;
#11648 = ORIENTED_EDGE ( 'NONE', *, *, #15922, .F. ) ;
#11649 = EDGE_LOOP ( 'NONE', ( #819, #3710, #14975, #5607 ) ) ;
#11650 = DIRECTION ( 'NONE',  ( -0.1566598588826321747, 0.9876526153536343555, 0.000000000000000000 ) ) ;
#11651 = ORIENTED_EDGE ( 'NONE', *, *, #1419, .T. ) ;
#11652 = DIRECTION ( 'NONE',  ( -0.1566598588826321192, 0.9876526153536342445, 7.798540720466730171E-17 ) ) ;
#11653 = CARTESIAN_POINT ( 'NONE',  ( -9.997901389864651378, -21.83563668437698269, 8.660254037844413944 ) ) ;
#11654 = ORIENTED_EDGE ( 'NONE', *, *, #8761, .T. ) ;
#11655 = CIRCLE ( 'NONE', #16525, 1.500000000000000000 ) ;
#11656 = VECTOR ( 'NONE', #5507, 1000.000000000000000 ) ;
#11657 = DIRECTION ( 'NONE',  ( -0.9876526153536341335, -0.1566598588826327021, 0.000000000000000000 ) ) ;
#11658 = EDGE_CURVE ( 'NONE', #10862, #8789, #18477, .T. ) ;
#11659 = EDGE_CURVE ( 'NONE', #6405, #5249, #13338, .T. ) ;
#11660 = CARTESIAN_POINT ( 'NONE',  ( -170.4124675745486570, 31.54971992778987655, 2.500000000000000000 ) ) ;
#11661 = LINE ( 'NONE', #16061, #14534 ) ;
#11662 = ADVANCED_FACE ( 'NONE', ( #15905 ), #5955, .F. ) ;
#11663 = DIRECTION ( 'NONE',  ( -0.1566598588826321747, 0.9876526153536343555, 0.000000000000000000 ) ) ;
#11664 = ORIENTED_EDGE ( 'NONE', *, *, #18096, .F. ) ;
#11665 = ORIENTED_EDGE ( 'NONE', *, *, #8423, .F. ) ;
#11666 = FACE_BOUND ( 'NONE', #6113, .T. ) ;
#11667 = CIRCLE ( 'NONE', #15926, 12.74754878398196567 ) ;
#11668 = CARTESIAN_POINT ( 'NONE',  ( -89.99999999999998579, -35.00000000000001421, -35.00000000000000000 ) ) ;
#11669 = DIRECTION ( 'NONE',  ( 0.000000000000000000, 0.000000000000000000, 1.000000000000000000 ) ) ;
#11670 = AXIS2_PLACEMENT_3D ( 'NONE', #14765, #3278, #9078 ) ;
#11671 = VERTEX_POINT ( 'NONE', #2909 ) ;
#11672 = VERTEX_POINT ( 'NONE', #14671 ) ;
#11673 = DIRECTION ( 'NONE',  ( 0.000000000000000000, 0.000000000000000000, 1.000000000000000000 ) ) ;
#11674 = AXIS2_PLACEMENT_3D ( 'NONE', #18514, #3744, #18415 ) ;
#11675 = DIRECTION ( 'NONE',  ( 0.000000000000000000, 0.000000000000000000, 1.000000000000000000 ) ) ;
#11676 = AXIS2_PLACEMENT_3D ( 'NONE', #14120, #15632, #14329 ) ;
#11677 = CARTESIAN_POINT ( 'NONE',  ( -44.56574292724170760, -27.31873174526908699, 8.660254037844417496 ) ) ;
#11678 = FACE_OUTER_BOUND ( 'NONE', #3625, .T. ) ;
#11679 = EDGE_CURVE ( 'NONE', #8810, #1168, #16315, .T. ) ;
#11680 = EDGE_CURVE ( 'NONE', #11588, #15928, #11140, .T. ) ;
#11681 = CARTESIAN_POINT ( 'NONE',  ( -31.68662391746665463, -82.98133501614300656, 21.65063509461101532 ) ) ;
#11682 = AXIS2_PLACEMENT_3D ( 'NONE', #16261, #1948, #533 ) ;
#11683 = CARTESIAN_POINT ( 'NONE',  ( 55.85952145814821534, 6.938893903907228378E-15, 30.00000000000000000 ) ) ;
#11684 = VECTOR ( 'NONE', #14680, 1000.000000000000000 ) ;
#11685 = CARTESIAN_POINT ( 'NONE',  ( -77.65210554158829837, -32.56683701783724416, 8.660254037844417496 ) ) ;
#11686 = DIRECTION ( 'NONE',  ( -1.000000000000000000, 0.000000000000000000, 0.000000000000000000 ) ) ;
#11687 = VERTEX_POINT ( 'NONE', #13060 ) ;
#11688 = CARTESIAN_POINT ( 'NONE',  ( -57.69469991357524208, -24.33871690453384673, -12.99038105676658006 ) ) ;
#11689 = ORIENTED_EDGE ( 'NONE', *, *, #7756, .T. ) ;
#11690 = CIRCLE ( 'NONE', #8394, 1.500000000000001332 ) ;
#11691 = ORIENTED_EDGE ( 'NONE', *, *, #6366, .F. ) ;
#11692 = EDGE_CURVE ( 'NONE', #4161, #3161, #2975, .T. ) ;
#11693 = ORIENTED_EDGE ( 'NONE', *, *, #6000, .F. ) ;
#11694 = AXIS2_PLACEMENT_3D ( 'NONE', #663, #6450, #12186 ) ;
#11695 = ORIENTED_EDGE ( 'NONE', *, *, #13598, .F. ) ;
#11696 = CARTESIAN_POINT ( 'NONE',  ( -61.15148406731293562, -24.88702641062306142, -4.330127018922180326 ) ) ;
#11697 = ORIENTED_EDGE ( 'NONE', *, *, #16058, .F. ) ;
#11698 = ORIENTED_EDGE ( 'NONE', *, *, #6747, .T. ) ;
#11699 = LINE ( 'NONE', #8888, #18256 ) ;
#11700 = AXIS2_PLACEMENT_3D ( 'NONE', #4941, #1936, #17893 ) ;
#11701 = FACE_OUTER_BOUND ( 'NONE', #9205, .T. ) ;
#11702 = DIRECTION ( 'NONE',  ( -0.1566598588826321192, 0.9876526153536342445, 7.798540720466730171E-17 ) ) ;
#11703 = CARTESIAN_POINT ( 'NONE',  ( -47.03487446562577645, -27.71038139247565368, 4.330127018922217630 ) ) ;
#11704 = CYLINDRICAL_SURFACE ( 'NONE', #10047, 1.500000000000000666 ) ;
#11705 = DIRECTION ( 'NONE',  ( -0.9201637183752249260, -0.3915338189555018777, 0.000000000000000000 ) ) ;
#11706 = DIRECTION ( 'NONE',  ( -0.1566598588826321192, 0.9876526153536342445, 7.798540720466730171E-17 ) ) ;
#11707 = ORIENTED_EDGE ( 'NONE', *, *, #13670, .T. ) ;
#11708 = FACE_OUTER_BOUND ( 'NONE', #11027, .T. ) ;
#11709 = DIRECTION ( 'NONE',  ( 1.000000000000000000, 0.000000000000000000, -0.000000000000000000 ) ) ;
#11711 = ORIENTED_EDGE ( 'NONE', *, *, #8952, .T. ) ;
#11710 = DIRECTION ( 'NONE',  ( -0.9876526153536336894, -0.1566598588826349503, 0.000000000000000000 ) ) ;
#11712 = ADVANCED_FACE ( 'NONE', ( #11802 ), #17650, .T. ) ;
#11713 = AXIS2_PLACEMENT_3D ( 'NONE', #12399, #13916, #16698 ) ;
#11714 = ORIENTED_EDGE ( 'NONE', *, *, #9681, .T. ) ;
#11715 = EDGE_CURVE ( 'NONE', #15259, #18385, #4705, .T. ) ;
#11716 = CARTESIAN_POINT ( 'NONE',  ( -138.4775067298212718, -42.93618108924343346, -2.500000000000000000 ) ) ;
#11717 = ORIENTED_EDGE ( 'NONE', *, *, #6776, .F. ) ;
#11718 = EDGE_LOOP ( 'NONE', ( #6866, #5058, #2935, #17155 ) ) ;
#11719 = DIRECTION ( 'NONE',  ( 0.000000000000000000, 0.000000000000000000, 1.000000000000000000 ) ) ;
#11720 = ADVANCED_FACE ( 'NONE', ( #16478 ), #10753, .F. ) ;
#11721 = AXIS2_PLACEMENT_3D ( 'NONE', #16679, #2247, #2162 ) ;
#11722 = VERTEX_POINT ( 'NONE', #13418 ) ;
#11723 = DIRECTION ( 'NONE',  ( -0.1566598588826321192, 0.9876526153536342445, 7.798540720466730171E-17 ) ) ;
#11724 = VECTOR ( 'NONE', #3483, 1000.000000000000000 ) ;
#11725 = CIRCLE ( 'NONE', #16619, 1.500000000000000888 ) ;
#11726 = CARTESIAN_POINT ( 'NONE',  ( -76.90684458043445204, -2.166085715380211774, -7.123062958295337310 ) ) ;
#11727 = ORIENTED_EDGE ( 'NONE', *, *, #4633, .F. ) ;
#11728 = DIRECTION ( 'NONE',  ( 0.000000000000000000, 0.000000000000000000, 1.000000000000000000 ) ) ;
#11729 = ORIENTED_EDGE ( 'NONE', *, *, #2847, .F. ) ;
#11730 = DIRECTION ( 'NONE',  ( -0.9876526153536344665, -0.1566598588826304539, 0.000000000000000000 ) ) ;
#11731 = CIRCLE ( 'NONE', #16947, 1.499999999999999556 ) ;
#11732 = CARTESIAN_POINT ( 'NONE',  ( -30.20514499443620338, -82.74634522781903456, -4.330127018922185655 ) ) ;
#11733 = CIRCLE ( 'NONE', #3570, 1.500000000000000888 ) ;
#11734 = DIRECTION ( 'NONE',  ( 0.000000000000000000, 0.000000000000000000, 1.000000000000000000 ) ) ;
#11735 = EDGE_LOOP ( 'NONE', ( #1434, #17225 ) ) ;
#11736 = CIRCLE ( 'NONE', #16003, 1.500000000000001332 ) ;
#11737 = ORIENTED_EDGE ( 'NONE', *, *, #18785, .F. ) ;
#11738 = ORIENTED_EDGE ( 'NONE', *, *, #12148, .T. ) ;
#11739 = ORIENTED_EDGE ( 'NONE', *, *, #2372, .F. ) ;
#11740 = CARTESIAN_POINT ( 'NONE',  ( -129.1404785418517918, 52.54032238931508658, 2.500000000000000000 ) ) ;
#11741 = ADVANCED_FACE ( 'NONE', ( #10483 ), #16278, .F. ) ;
#11742 = VERTEX_POINT ( 'NONE', #3553 ) ;
#11743 = CARTESIAN_POINT ( 'NONE',  ( -33.16810284049712010, -83.21632480446695013, -21.65063509461098690 ) ) ;
#11744 = DIRECTION ( 'NONE',  ( -0.1566598588826321192, 0.9876526153536342445, 7.798540720466731404E-17 ) ) ;
#11745 = ORIENTED_EDGE ( 'NONE', *, *, #7518, .T. ) ;
#11746 = AXIS2_PLACEMENT_3D ( 'NONE', #13928, #981, #6753 ) ;
#11747 = ORIENTED_EDGE ( 'NONE', *, *, #8633, .T. ) ;
#11748 = EDGE_CURVE ( 'NONE', #13719, #3635, #13786, .T. ) ;
#11749 = AXIS2_PLACEMENT_3D ( 'NONE', #7946, #656, #12081 ) ;
#11750 = ORIENTED_EDGE ( 'NONE', *, *, #4671, .T. ) ;
#11751 = ORIENTED_EDGE ( 'NONE', *, *, #3998, .T. ) ;
#11752 = DIRECTION ( 'NONE',  ( -0.1566598588826321192, 0.9876526153536342445, 7.798540720466730171E-17 ) ) ;
#11753 = DIRECTION ( 'NONE',  ( 8.693966348389027220E-17, -1.991237296706374949E-16, 1.000000000000000000 ) ) ;
#11754 = DIRECTION ( 'NONE',  ( -0.1566598588826321747, 0.9876526153536343555, 0.000000000000000000 ) ) ;
#11755 = AXIS2_PLACEMENT_3D ( 'NONE', #14921, #524, #12445 ) ;
#11756 = CARTESIAN_POINT ( 'NONE',  ( -72.30733464426469936, 45.98178131438659477, -3.159861247684372820 ) ) ;
#11757 = ORIENTED_EDGE ( 'NONE', *, *, #12952, .F. ) ;
#11758 = ORIENTED_EDGE ( 'NONE', *, *, #3719, .F. ) ;
#11759 = CARTESIAN_POINT ( 'NONE',  ( -25.59598991458226536, -19.24727149084831979, -8.660254037844380193 ) ) ;
#11760 = EDGE_CURVE ( 'NONE', #5727, #8327, #11733, .T. ) ;
#11761 = AXIS2_PLACEMENT_3D ( 'NONE', #6004, #1732, #7626 ) ;
#11762 = VERTEX_POINT ( 'NONE', #4798 ) ;
#11763 = DIRECTION ( 'NONE',  ( 0.000000000000000000, 0.000000000000000000, 1.000000000000000000 ) ) ;
#11764 = CARTESIAN_POINT ( 'NONE',  ( -12.46703292824872733, -22.22728633158356359, 4.330127018922214077 ) ) ;
#11765 = AXIS2_PLACEMENT_3D ( 'NONE', #10734, #532, #16460 ) ;
#11766 = EDGE_CURVE ( 'NONE', #14764, #4082, #4975, .T. ) ;
#11767 = CIRCLE ( 'NONE', #12063, 1.500000000000000888 ) ;
#11768 = AXIS2_PLACEMENT_3D ( 'NONE', #12992, #2853, #18653 ) ;
#11769 = ORIENTED_EDGE ( 'NONE', *, *, #5449, .T. ) ;
#11770 = FACE_OUTER_BOUND ( 'NONE', #15533, .T. ) ;
#11771 = EDGE_CURVE ( 'NONE', #755, #13426, #8023, .T. ) ;
#11772 = AXIS2_PLACEMENT_3D ( 'NONE', #8378, #5549, #15862 ) ;
#11773 = CIRCLE ( 'NONE', #3597, 1.500000000000000888 ) ;
#11774 = CARTESIAN_POINT ( 'NONE',  ( -11.93357161039406300, -79.84813783849037350, 21.65063509461100821 ) ) ;
#11775 = DIRECTION ( 'NONE',  ( -0.1566598588826321192, 0.9876526153536342445, 7.798540720466730171E-17 ) ) ;
#11776 = EDGE_LOOP ( 'NONE', ( #5882, #5273, #3994, #11148 ) ) ;
#11777 = AXIS2_PLACEMENT_3D ( 'NONE', #789, #13945, #11187 ) ;
#11778 = DIRECTION ( 'NONE',  ( -0.1566598588826321192, 0.9876526153536342445, 7.798540720466730171E-17 ) ) ;
#11779 = AXIS2_PLACEMENT_3D ( 'NONE', #9761, #6922, #15527 ) ;
#11780 = CARTESIAN_POINT ( 'NONE',  ( 7.819480696678551723, -76.71494066083772623, 21.65063509461100821 ) ) ;
#11781 = CARTESIAN_POINT ( 'NONE',  ( -19.34096622554629263, -81.02308678011010556, 17.32050807568881368 ) ) ;
#11782 = CARTESIAN_POINT ( 'NONE',  ( 0.000000000000000000, 0.000000000000000000, 25.00000000000000000 ) ) ;
#11783 = ORIENTED_EDGE ( 'NONE', *, *, #6849, .F. ) ;
#11784 = ORIENTED_EDGE ( 'NONE', *, *, #4207, .T. ) ;
#11785 = FACE_OUTER_BOUND ( 'NONE', #9004, .T. ) ;
#11786 = EDGE_CURVE ( 'NONE', #18596, #8019, #14855, .T. ) ;
#11787 = ORIENTED_EDGE ( 'NONE', *, *, #6843, .F. ) ;
#11788 = ORIENTED_EDGE ( 'NONE', *, *, #1330, .T. ) ;
#11789 = AXIS2_PLACEMENT_3D ( 'NONE', #1364, #2671, #8648 ) ;
#11790 = ORIENTED_EDGE ( 'NONE', *, *, #4064, .T. ) ;
#11791 = EDGE_CURVE ( 'NONE', #4290, #7926, #15103, .T. ) ;
#11792 = EDGE_CURVE ( 'NONE', #13882, #15648, #16636, .T. ) ;
#11793 = EDGE_CURVE ( 'NONE', #15439, #16580, #9667, .T. ) ;
#11794 = CIRCLE ( 'NONE', #5785, 1.500000000000001332 ) ;
#11795 = CARTESIAN_POINT ( 'NONE',  ( -37.94164760650263446, -21.20551972688122788, 21.65063509461101887 ) ) ;
#11796 = VECTOR ( 'NONE', #10172, 1000.000000000000000 ) ;
#11797 = CARTESIAN_POINT ( 'NONE',  ( -8.476787456656362352, -79.29982833240116236, 21.65063509461100821 ) ) ;
#11798 = DIRECTION ( 'NONE',  ( -0.1566598588826321192, 0.9876526153536342445, 7.798540720466731404E-17 ) ) ;
#11799 = CARTESIAN_POINT ( 'NONE',  ( -49.01017969633301874, -28.02370111024092481, 21.65063509461101887 ) ) ;
#11800 = SURFACE_SIDE_STYLE ('',( #12079 ) ) ;
#11801 = AXIS2_PLACEMENT_3D ( 'NONE', #6024, #14924, #16360 ) ;
#11802 = FACE_OUTER_BOUND ( 'NONE', #12093, .T. ) ;
#11803 = VERTEX_POINT ( 'NONE', #1879 ) ;
#11804 = AXIS2_PLACEMENT_3D ( 'NONE', #2895, #18784, #13220 ) ;
#11805 = DIRECTION ( 'NONE',  ( -0.1566598588826321192, 0.9876526153536342445, 7.798540720466731404E-17 ) ) ;
#11806 = CARTESIAN_POINT ( 'NONE',  ( -6.047290928450125946, -21.20899724884646531, -4.330127018922184767 ) ) ;
#11807 = ORIENTED_EDGE ( 'NONE', *, *, #17686, .F. ) ;
#11808 = DIRECTION ( 'NONE',  ( -0.1566598588826321192, 0.9876526153536342445, 7.798540720466731404E-17 ) ) ;
#11810 = ORIENTED_EDGE ( 'NONE', *, *, #4297, .T. ) ;
#11809 = DIRECTION ( 'NONE',  ( -0.9876526153536341335, -0.1566598588826327021, 0.000000000000000000 ) ) ;
#11811 = VERTEX_POINT ( 'NONE', #7671 ) ;
#11812 = ORIENTED_EDGE ( 'NONE', *, *, #3818, .F. ) ;
#11813 = FACE_OUTER_BOUND ( 'NONE', #1348, .T. ) ;
#11814 = VERTEX_POINT ( 'NONE', #9456 ) ;
#11815 = VECTOR ( 'NONE', #14307, 1000.000000000000000 ) ;
#11816 = ORIENTED_EDGE ( 'NONE', *, *, #519, .T. ) ;
#11817 = AXIS2_PLACEMENT_3D ( 'NONE', #8534, #8621, #14309 ) ;
#11818 = ORIENTED_EDGE ( 'NONE', *, *, #12705, .F. ) ;
#11819 = CARTESIAN_POINT ( 'NONE',  ( -22.79775037928398618, -81.57139628619930249, -8.660254037844385522 ) ) ;
#11820 = ORIENTED_EDGE ( 'NONE', *, *, #2271, .T. ) ;
#11821 = DIRECTION ( 'NONE',  ( -0.1566598588826321192, 0.9876526153536342445, 7.798540720466730171E-17 ) ) ;
#11822 = ORIENTED_EDGE ( 'NONE', *, *, #6025, .T. ) ;
#11823 = DIRECTION ( 'NONE',  ( -0.1566598588826321747, 0.9876526153536343555, 0.000000000000000000 ) ) ;
#11824 = DIRECTION ( 'NONE',  ( -0.9876526153536336894, -0.1566598588826349503, 0.000000000000000000 ) ) ;
#11825 = ORIENTED_EDGE ( 'NONE', *, *, #434, .F. ) ;
#11826 = EDGE_CURVE ( 'NONE', #5678, #12283, #1499, .T. ) ;
#11827 = AXIS2_PLACEMENT_3D ( 'NONE', #8848, #15655, #41 ) ;
#11828 = ADVANCED_FACE ( 'NONE', ( #18017 ), #15228, .F. ) ;
#11829 = B_SPLINE_CURVE_WITH_KNOTS ( 'NONE', 3,
 ( #18383, #4097, #11110, #14059 ),
 .UNSPECIFIED., .F., .F.,
 ( 4, 4 ),
 ( 0.000000000000000000, 0.003000475340473869428 ),
 .UNSPECIFIED. ) ;
#11830 = CARTESIAN_POINT ( 'NONE',  ( -31.68662391746666884, -82.98133501614299234, -21.65063509461098690 ) ) ;
#11831 = VERTEX_POINT ( 'NONE', #3372 ) ;
#11832 = FACE_BOUND ( 'NONE', #115, .T. ) ;
#11833 = VECTOR ( 'NONE', #17097, 1000.000000000000000 ) ;
#11834 = DIRECTION ( 'NONE',  ( 0.2388812686885108949, 0.9710487832595062763, 1.725905983023835105E-16 ) ) ;
#11835 = ORIENTED_EDGE ( 'NONE', *, *, #1956, .T. ) ;
#11836 = CARTESIAN_POINT ( 'NONE',  ( -64.20000000000000284, 2.694222958124175527E-16, -25.00000000000000000 ) ) ;
#11837 = CARTESIAN_POINT ( 'NONE',  ( 4.362696542940843081, -77.26325016692693737, -4.330127018922189208 ) ) ;
#11838 = VERTEX_POINT ( 'NONE', #9177 ) ;
#11839 = ORIENTED_EDGE ( 'NONE', *, *, #9023, .T. ) ;
#11840 = ORIENTED_EDGE ( 'NONE', *, *, #12963, .F. ) ;
#11841 = ORIENTED_EDGE ( 'NONE', *, *, #7332, .F. ) ;
#11842 = EDGE_LOOP ( 'NONE', ( #234, #6773 ) ) ;
#11843 = CARTESIAN_POINT ( 'NONE',  ( -175.0529311237955881, 56.11526690008648899, -2.500000000000065725 ) ) ;
#11844 = ORIENTED_EDGE ( 'NONE', *, *, #7288, .T. ) ;
#11845 = ORIENTED_EDGE ( 'NONE', *, *, #13427, .T. ) ;
#11846 = FACE_BOUND ( 'NONE', #14227, .T. ) ;
#11847 =( GEOMETRIC_REPRESENTATION_CONTEXT ( 3 ) GLOBAL_UNCERTAINTY_ASSIGNED_CONTEXT ( ( #1899 ) ) GLOBAL_UNIT_ASSIGNED_CONTEXT ( ( #7601, #194, #4457 ) ) REPRESENTATION_CONTEXT ( 'NONE', 'WORKASPACE' ) );
#11848 = DIRECTION ( 'NONE',  ( -0.000000000000000000, -1.000000000000000000, -0.000000000000000000 ) ) ;
#11849 = EDGE_LOOP ( 'NONE', ( #8861, #7919 ) ) ;
#11850 = FACE_OUTER_BOUND ( 'NONE', #17435, .T. ) ;
#11851 = ORIENTED_EDGE ( 'NONE', *, *, #169, .F. ) ;
#11852 = EDGE_CURVE ( 'NONE', #3442, #10192, #14947, .T. ) ;
#11853 = VECTOR ( 'NONE', #16433, 1000.000000000000000 ) ;
#11854 = EDGE_CURVE ( 'NONE', #1643, #4960, #17870, .T. ) ;
#11855 = ORIENTED_EDGE ( 'NONE', *, *, #17021, .F. ) ;
#11856 = ADVANCED_FACE ( 'NONE', ( #4896, #12182 ), #16780, .T. ) ;
#11857 = CARTESIAN_POINT ( 'NONE',  ( -44.07191661956487394, -27.24040181582776299, 4.330127018922217630 ) ) ;
#11858 = LINE ( 'NONE', #6301, #1225 ) ;
#11859 = CYLINDRICAL_SURFACE ( 'NONE', #9340, 1.500000000000001554 ) ;
#11860 = CARTESIAN_POINT ( 'NONE',  ( -18.35331361019266794, -80.86642692122747178, -12.99038105676658539 ) ) ;
#11861 = VERTEX_POINT ( 'NONE', #18510 ) ;
#11862 = VERTEX_POINT ( 'NONE', #18317 ) ;
#11863 = CARTESIAN_POINT ( 'NONE',  ( -129.1404785418517918, -2.850701963179328668, 9.951701414186818625E-16 ) ) ;
#11864 = DIRECTION ( 'NONE',  ( -0.1566598588826321192, 0.9876526153536342445, 7.798540720466731404E-17 ) ) ;
#11865 = CARTESIAN_POINT ( 'NONE',  ( -63.62061560569701157, -25.27867605782963523, -17.32050807568878170 ) ) ;
#11866 = AXIS2_PLACEMENT_3D ( 'NONE', #17946, #10695, #7865 ) ;
#11867 = ORIENTED_EDGE ( 'NONE', *, *, #4266, .T. ) ;
#11868 = DIRECTION ( 'NONE',  ( -0.9876526153536336894, -0.1566598588826350336, 0.000000000000000000 ) ) ;
#11869 = CARTESIAN_POINT ( 'NONE',  ( -21.64537945316773460, -18.62063205531779531, -4.330127018922180326 ) ) ;
#11870 = CARTESIAN_POINT ( 'NONE',  ( -65.23030399291528170, -43.49999999999991473, 110.7545852194966045 ) ) ;
#11871 = DIRECTION ( 'NONE',  ( 0.000000000000000000, 0.000000000000000000, 1.000000000000000000 ) ) ;
#11872 = ORIENTED_EDGE ( 'NONE', *, *, #9131, .F. ) ;
#11873 = EDGE_CURVE ( 'NONE', #18049, #13271, #15714, .T. ) ;
#11874 = CARTESIAN_POINT ( 'NONE',  ( -45.55339554259533230, -27.47539160415171722, -4.330127018922181215 ) ) ;
#11875 = FILL_AREA_STYLE ('',( #14839 ) ) ;
#11876 = CARTESIAN_POINT ( 'NONE',  ( -61.15148406731292852, -24.88702641062306853, 12.99038105676661736 ) ) ;
#11877 = EDGE_LOOP ( 'NONE', ( #12533, #12707, #3773, #17180 ) ) ;
#11878 = ORIENTED_EDGE ( 'NONE', *, *, #1933, .T. ) ;
#11879 = DIRECTION ( 'NONE',  ( -0.9876526153536336894, -0.1566598588826349503, 0.000000000000000000 ) ) ;
#11880 = ORIENTED_EDGE ( 'NONE', *, *, #9840, .T. ) ;
#11881 = ADVANCED_FACE ( 'NONE', ( #8319 ), #18609, .F. ) ;
#11882 = ORIENTED_EDGE ( 'NONE', *, *, #12943, .F. ) ;
#11883 = VERTEX_POINT ( 'NONE', #5479 ) ;
#11884 = CIRCLE ( 'NONE', #7690, 145.0000000000000284 ) ;
#11885 = LINE ( 'NONE', #15313, #8975 ) ;
#11886 = DIRECTION ( 'NONE',  ( -0.5989998693185457634, -0.8007491221077704946, -1.362228425344026962E-16 ) ) ;
#11887 = DIRECTION ( 'NONE',  ( 0.000000000000000000, 0.000000000000000000, 1.000000000000000000 ) ) ;
#11888 = LINE ( 'NONE', #4796, #9150 ) ;
#11889 = CARTESIAN_POINT ( 'NONE',  ( -22.63303206852135929, -18.77729191420042554, -17.32050807568878170 ) ) ;
#11890 = VERTEX_POINT ( 'NONE', #5573 ) ;
#11891 = CARTESIAN_POINT ( 'NONE',  ( -57.89905323451571206, -29.43363984018462176, -8.660254037844380193 ) ) ;
#11892 = EDGE_CURVE ( 'NONE', #13882, #2681, #4117, .T. ) ;
#11893 = FACE_OUTER_BOUND ( 'NONE', #12393, .T. ) ;
#11894 = VERTEX_POINT ( 'NONE', #9831 ) ;
#11895 = EDGE_CURVE ( 'NONE', #11990, #5990, #15420, .T. ) ;
#11897 = VERTEX_POINT ( 'NONE', #3833 ) ;
#11896 = CARTESIAN_POINT ( 'NONE',  ( -9.997901389864651378, -21.83563668437698269, 17.32050807568881012 ) ) ;
#11898 = EDGE_CURVE ( 'NONE', #211, #14889, #2400, .T. ) ;
#11899 = ORIENTED_EDGE ( 'NONE', *, *, #10161, .T. ) ;
#11900 = DIRECTION ( 'NONE',  ( -0.9876526153536341335, -0.1566598588826327021, 0.000000000000000000 ) ) ;
#11901 = ORIENTED_EDGE ( 'NONE', *, *, #2803, .F. ) ;
#11902 = ORIENTED_EDGE ( 'NONE', *, *, #10213, .F. ) ;
#11903 = CARTESIAN_POINT ( 'NONE',  ( -14.93616446663280328, -22.61893597879013740, 17.32050807568881012 ) ) ;
#11904 = FACE_OUTER_BOUND ( 'NONE', #2149, .T. ) ;
#11905 = DIRECTION ( 'NONE',  ( -0.9876526153536341335, -0.1566598588826327021, 0.000000000000000000 ) ) ;
#11906 = FACE_BOUND ( 'NONE', #15307, .T. ) ;
#11907 = UNCERTAINTY_MEASURE_WITH_UNIT (LENGTH_MEASURE( 1.000000000000000082E-05 ), #13122, 'distance_accuracy_value', 'NONE');
#11908 = DIRECTION ( 'NONE',  ( -0.9826218788918642533, -0.1856185419698762884, 0.000000000000000000 ) ) ;
#11909 = CARTESIAN_POINT ( 'NONE',  ( -84.16561914167408531, 33.59999999999999432, 25.00000000000001776 ) ) ;
#11910 = AXIS2_PLACEMENT_3D ( 'NONE', #4647, #10424, #16218 ) ;
#11911 = DIRECTION ( 'NONE',  ( -0.1566598588826321192, 0.9876526153536342445, 7.798540720466730171E-17 ) ) ;
#11912 = ORIENTED_EDGE ( 'NONE', *, *, #7868, .T. ) ;
#11913 = ADVANCED_FACE ( 'NONE', ( #14087 ), #15693, .F. ) ;
#11914 = DIRECTION ( 'NONE',  ( 0.000000000000000000, 0.000000000000000000, 1.000000000000000000 ) ) ;
#11915 = EDGE_LOOP ( 'NONE', ( #3131, #6899, #2815, #14212 ) ) ;
#11916 = DIRECTION ( 'NONE',  ( -0.1566598588826321192, 0.9876526153536342445, 7.798540720466730171E-17 ) ) ;
#11917 = LINE ( 'NONE', #14698, #3286 ) ;
#11918 = ORIENTED_EDGE ( 'NONE', *, *, #16936, .T. ) ;
#11919 = ORIENTED_EDGE ( 'NONE', *, *, #7495, .F. ) ;
#11920 = EDGE_LOOP ( 'NONE', ( #16927, #13448 ) ) ;
#11921 = CARTESIAN_POINT ( 'NONE',  ( -43.86756329862440396, -22.14547888017700927, 1.908195823574487804E-14 ) ) ;
#11922 = ORIENTED_EDGE ( 'NONE', *, *, #13766, .F. ) ;
#11923 = AXIS2_PLACEMENT_3D ( 'NONE', #14929, #12346, #7827 ) ;
#11924 = FACE_BOUND ( 'NONE', #4646, .T. ) ;
#11925 = ORIENTED_EDGE ( 'NONE', *, *, #1471, .F. ) ;
#11926 = ORIENTED_EDGE ( 'NONE', *, *, #6876, .F. ) ;
#11927 = VERTEX_POINT ( 'NONE', #15422 ) ;
#11928 = CARTESIAN_POINT ( 'NONE',  ( -90.00000000000000000, 34.99999999999999289, -35.00000000000000000 ) ) ;
#11929 = DIRECTION ( 'NONE',  ( 0.000000000000000000, 0.000000000000000000, 1.000000000000000000 ) ) ;
#11930 = CIRCLE ( 'NONE', #4077, 1.499999999999999556 ) ;
#11931 = CARTESIAN_POINT ( 'NONE',  ( -15.92381708198643153, -22.77559583767277473, 4.330127018922217630 ) ) ;
#11932 = DIRECTION ( 'NONE',  ( 0.000000000000000000, 0.000000000000000000, 1.000000000000000000 ) ) ;
#11933 = LINE ( 'NONE', #9032, #14998 ) ;
#11934 = EDGE_LOOP ( 'NONE', ( #8818, #6187, #13892, #6805 ) ) ;
#11935 = ORIENTED_EDGE ( 'NONE', *, *, #5461, .F. ) ;
#11936 = CYLINDRICAL_SURFACE ( 'NONE', #5411, 1.500000000000001554 ) ;
#11937 = FACE_OUTER_BOUND ( 'NONE', #4438, .T. ) ;
#11938 = ADVANCED_FACE ( 'NONE', ( #15597 ), #14185, .F. ) ;
#11939 = CARTESIAN_POINT ( 'NONE',  ( -39.91695283720987675, -21.51883944464649190, 12.99038105676661736 ) ) ;
#11940 = EDGE_LOOP ( 'NONE', ( #4118, #10489, #5098, #13728 ) ) ;
#11941 = EDGE_LOOP ( 'NONE', ( #18058, #17284 ) ) ;
#11942 = ADVANCED_FACE ( 'NONE', ( #13896 ), #944, .F. ) ;
#11943 = AXIS2_PLACEMENT_3D ( 'NONE', #17196, #15755, #8176 ) ;
#11944 = ORIENTED_EDGE ( 'NONE', *, *, #5223, .F. ) ;
#11945 = DIRECTION ( 'NONE',  ( -1.000000000000000000, 0.000000000000000000, 0.000000000000000000 ) ) ;
#11946 = DIRECTION ( 'NONE',  ( -0.1566598588826321192, 0.9876526153536342445, 7.798540720466730171E-17 ) ) ;
#11947 = EDGE_CURVE ( 'NONE', #9479, #13518, #6654, .T. ) ;
#11948 = CARTESIAN_POINT ( 'NONE',  ( -25.10216360690543524, -19.16894156140700645, -12.99038105676658006 ) ) ;
#11949 = CARTESIAN_POINT ( 'NONE',  ( -28.22983976372896109, -82.43302551005379541, 4.330127018922213189 ) ) ;
#11950 = DIRECTION ( 'NONE',  ( 0.000000000000000000, 0.000000000000000000, 1.000000000000000000 ) ) ;
#11951 =( NAMED_UNIT ( * ) PLANE_ANGLE_UNIT ( ) SI_UNIT ( $, .RADIAN. ) );
#11952 = ORIENTED_EDGE ( 'NONE', *, *, #17752, .F. ) ;
#11953 = AXIS2_PLACEMENT_3D ( 'NONE', #8846, #206, #17583 ) ;
#11954 = CARTESIAN_POINT ( 'NONE',  ( -68.72359699322777260, -88.85607972424168111, -8.660254037844385522 ) ) ;
#11955 = DIRECTION ( 'NONE',  ( 1.000000000000000000, 0.000000000000000000, 0.000000000000000000 ) ) ;
#11956 = CARTESIAN_POINT ( 'NONE',  ( -3.000000000000000000, 4.898587196589412829E-16, 37.00000000000000711 ) ) ;
#11957 = CARTESIAN_POINT ( 'NONE',  ( -47.03487446562577645, -27.71038139247565368, 12.99038105676661736 ) ) ;
#11958 = ORIENTED_EDGE ( 'NONE', *, *, #3645, .T. ) ;
#11959 = ORIENTED_EDGE ( 'NONE', *, *, #14184, .F. ) ;
#11960 = CARTESIAN_POINT ( 'NONE',  ( -0.1213752363283457369, -20.26903809555066616, 1.348786077179112100E-14 ) ) ;
#11961 = AXIS2_PLACEMENT_3D ( 'NONE', #14292, #2818, #1404 ) ;
#11962 = ORIENTED_EDGE ( 'NONE', *, *, #6807, .T. ) ;
#11963 = DIRECTION ( 'NONE',  ( -0.1566598588826321192, 0.9876526153536342445, 7.798540720466731404E-17 ) ) ;
#11964 = ORIENTED_EDGE ( 'NONE', *, *, #14218, .T. ) ;
#11965 = CIRCLE ( 'NONE', #3804, 1.500000000000000444 ) ;
#11966 = EDGE_CURVE ( 'NONE', #1641, #10341, #10258, .T. ) ;
#11967 = CARTESIAN_POINT ( 'NONE',  ( -26.58364252993588650, -19.40393134973095357, -12.99038105676658006 ) ) ;
#11968 = VERTEX_POINT ( 'NONE', #13998 ) ;
#11969 = CARTESIAN_POINT ( 'NONE',  ( -62.83731631128386397, -30.21693913459777647, -17.32050807568878170 ) ) ;
#11970 = ORIENTED_EDGE ( 'NONE', *, *, #14923, .T. ) ;
#11971 = CARTESIAN_POINT ( 'NONE',  ( -35.14340807120436239, -83.52964452223220349, -4.330127018922185655 ) ) ;
#11972 = CARTESIAN_POINT ( 'NONE',  ( -81.73462711737164454, 33.01666666666666572, -35.00000000000000000 ) ) ;
#11973 = ADVANCED_FACE ( 'NONE', ( #12555 ), #18410, .F. ) ;
#11974 = AXIS2_PLACEMENT_3D ( 'NONE', #3469, #10864, #12488 ) ;
#11975 = CARTESIAN_POINT ( 'NONE',  ( -129.1404785418517918, -2.850701963179328668, 9.951701414186818625E-16 ) ) ;
#11976 = ORIENTED_EDGE ( 'NONE', *, *, #5595, .T. ) ;
#11977 = DIRECTION ( 'NONE',  ( 0.000000000000000000, 0.000000000000000000, 1.000000000000000000 ) ) ;
#11978 = FACE_BOUND ( 'NONE', #2523, .T. ) ;
#11979 = CIRCLE ( 'NONE', #9595, 1.500000000000000888 ) ;
#11980 = CARTESIAN_POINT ( 'NONE',  ( -176.1167811578620501, -139.6880237571007513, 2.500000000000000000 ) ) ;
#11981 = FACE_OUTER_BOUND ( 'NONE', #12446, .T. ) ;
#11982 = CARTESIAN_POINT ( 'NONE',  ( -0.5755665338273054932, -78.04654946134009208, 12.99038105676660848 ) ) ;
#11983 = CYLINDRICAL_SURFACE ( 'NONE', #9957, 149.4844750268700864 ) ;
#11985 = ORIENTED_EDGE ( 'NONE', *, *, #10037, .T. ) ;
#11984 = CARTESIAN_POINT ( 'NONE',  ( -46.50141314777111745, -85.33123289938248490, -4.330127018922185655 ) ) ;
#11986 = ORIENTED_EDGE ( 'NONE', *, *, #14705, .F. ) ;
#11987 = DIRECTION ( 'NONE',  ( -0.1566598588826321192, 0.9876526153536342445, 7.798540720466731404E-17 ) ) ;
#11988 = CIRCLE ( 'NONE', #12918, 1.500000000000001332 ) ;
#11989 = COLOUR_RGB ( '', 0.66274510, 0.83137255, 0.94901961) ;
#11990 = VERTEX_POINT ( 'NONE', #5382 ) ;
#11991 = CIRCLE ( 'NONE', #8701, 1.500000000000000000 ) ;
#11992 = ORIENTED_EDGE ( 'NONE', *, *, #6505, .F. ) ;
#11993 = CARTESIAN_POINT ( 'NONE',  ( -48.97054468615519340, -85.72288254658904805, -17.32050807568878525 ) ) ;
#11994 = ADVANCED_FACE ( 'NONE', ( #3937 ), #11136, .F. ) ;
#11995 = DIRECTION ( 'NONE',  ( -0.9876526153536336894, -0.1566598588826349503, 0.000000000000000000 ) ) ;
#11996 = CIRCLE ( 'NONE', #11694, 1.500000000000000888 ) ;
#11997 = EDGE_CURVE ( 'NONE', #2873, #15378, #7013, .T. ) ;
#11998 = CARTESIAN_POINT ( 'NONE',  ( -89.99999999999998579, -35.00000000000001421, -30.00000000000000000 ) ) ;
#11999 = CARTESIAN_POINT ( 'NONE',  ( -9.299721761247353058, -16.66238381928489787, 1.561251128379126385E-14 ) ) ;
#12000 = DIRECTION ( 'NONE',  ( 0.000000000000000000, 0.000000000000000000, 1.000000000000000000 ) ) ;
#12001 = ADVANCED_FACE ( 'NONE', ( #2982 ), #7550, .F. ) ;
#12002 = CARTESIAN_POINT ( 'NONE',  ( -128.1677737538113604, -15.15243288452917270, -3.279750847804472347 ) ) ;
#12003 = CARTESIAN_POINT ( 'NONE',  ( -11.76885329963143434, -17.05403346649147878, -12.99038105676658006 ) ) ;
#12004 = DIRECTION ( 'NONE',  ( -0.1566598588826321192, 0.9876526153536342445, 7.798540720466731404E-17 ) ) ;
#12005 = CARTESIAN_POINT ( 'NONE',  ( 10.28861223506262412, -76.32329101363113466, -17.32050807568878525 ) ) ;
#12006 = ORIENTED_EDGE ( 'NONE', *, *, #1735, .T. ) ;
#12007 = AXIS2_PLACEMENT_3D ( 'NONE', #7693, #13360, #13442 ) ;
#12008 = CARTESIAN_POINT ( 'NONE',  ( 4.362696542940843081, -77.26325016692693737, 21.65063509461100821 ) ) ;
#12009 = ORIENTED_EDGE ( 'NONE', *, *, #7441, .T. ) ;
#12010 = CARTESIAN_POINT ( 'NONE',  ( -12.92122422574768592, -80.00479769737299307, -8.660254037844385522 ) ) ;
#12011 = DIRECTION ( 'NONE',  ( -0.9876526153536336894, -0.1566598588826349503, 0.000000000000000000 ) ) ;
#12012 = AXIS2_PLACEMENT_3D ( 'NONE', #13343, #14673, #11709 ) ;
#12013 = LINE ( 'NONE', #13264, #18790 ) ;
#12014 = ORIENTED_EDGE ( 'NONE', *, *, #11076, .T. ) ;
#12015 = ORIENTED_EDGE ( 'NONE', *, *, #7836, .T. ) ;
#12016 = ORIENTED_EDGE ( 'NONE', *, *, #15105, .F. ) ;
#12017 = DIRECTION ( 'NONE',  ( 0.000000000000000000, 0.000000000000000000, -1.000000000000000000 ) ) ;
#12018 = AXIS2_PLACEMENT_3D ( 'NONE', #8664, #14265, #12826 ) ;
#12019 = ORIENTED_EDGE ( 'NONE', *, *, #12410, .F. ) ;
#12020 = FACE_BOUND ( 'NONE', #11567, .T. ) ;
#12021 = ADVANCED_FACE ( 'NONE', ( #18777 ), #7187, .F. ) ;
#12022 = STYLED_ITEM ( 'NONE', ( #4617 ), #16831 ) ;
#12023 = ADVANCED_FACE ( 'NONE', ( #5771 ), #17624, .F. ) ;
#12024 = ADVANCED_FACE ( 'NONE', ( #1495 ), #14465, .F. ) ;
#12025 = DIRECTION ( 'NONE',  ( -0.9876526153536336894, -0.1566598588826349503, 0.000000000000000000 ) ) ;
#12026 = ORIENTED_EDGE ( 'NONE', *, *, #14153, .F. ) ;
#12027 = VERTEX_POINT ( 'NONE', #7453 ) ;
#12028 = AXIS2_PLACEMENT_3D ( 'NONE', #9037, #6012, #17605 ) ;
#12029 = AXIS2_PLACEMENT_3D ( 'NONE', #11260, #18342, #14018 ) ;
#12030 = LINE ( 'NONE', #14633, #9145 ) ;
#12031 = CARTESIAN_POINT ( 'NONE',  ( -28.22983976372897530, -82.43302551005378120, -21.65063509461098690 ) ) ;
#12032 = AXIS2_PLACEMENT_3D ( 'NONE', #4485, #8753, #17599 ) ;
#12033 = DIRECTION ( 'NONE',  ( -0.000000000000000000, -0.000000000000000000, -1.000000000000000000 ) ) ;
#12034 = COLOUR_RGB ( '', 0.09019608, 0.27058824, 0.51372549) ;
#12035 = CARTESIAN_POINT ( 'NONE',  ( -57.89905323451569785, -29.43363984018461466, 8.660254037844417496 ) ) ;
#12036 = DIRECTION ( 'NONE',  ( 0.000000000000000000, -1.000000000000000000, 0.000000000000000000 ) ) ;
#12037 = DIRECTION ( 'NONE',  ( -0.9876526153536341335, -0.1566598588826327021, 0.000000000000000000 ) ) ;
#12038 = EDGE_LOOP ( 'NONE', ( #10457, #12120, #13851, #4456 ) ) ;
#12039 = ORIENTED_EDGE ( 'NONE', *, *, #15829, .T. ) ;
#12040 = CARTESIAN_POINT ( 'NONE',  ( -5.000000000000000000, 0.000000000000000000, -35.00000000000000000 ) ) ;
#12041 = CARTESIAN_POINT ( 'NONE',  ( -19.17624791478365864, -18.22898240811121795, 1.908195823574487804E-14 ) ) ;
#12042 = EDGE_CURVE ( 'NONE', #5315, #12777, #1756, .T. ) ;
#12043 = ORIENTED_EDGE ( 'NONE', *, *, #5725, .T. ) ;
#12044 = AXIS2_PLACEMENT_3D ( 'NONE', #4376, #2580, #17200 ) ;
#12045 = ORIENTED_EDGE ( 'NONE', *, *, #1694, .T. ) ;
#12046 = CARTESIAN_POINT ( 'NONE',  ( -65.26681283949008616, -88.30777021815246997, 1.424741226644455312E-14 ) ) ;
#12047 = AXIS2_PLACEMENT_3D ( 'NONE', #6814, #12757, #17144 ) ;
#12048 = CIRCLE ( 'NONE', #8462, 1.499999999999999556 ) ;
#12049 = DIRECTION ( 'NONE',  ( -0.1566598588826321192, 0.9876526153536342445, 7.798540720466730171E-17 ) ) ;
#12050 = DIRECTION ( 'NONE',  ( -0.000000000000000000, -0.000000000000000000, -1.000000000000000000 ) ) ;
#12051 = DIRECTION ( 'NONE',  ( -0.1566598588826321192, 0.9876526153536342445, 7.798540720466730171E-17 ) ) ;
#12052 = EDGE_CURVE ( 'NONE', #14468, #299, #2987, .T. ) ;
#12053 = VERTEX_POINT ( 'NONE', #11508 ) ;
#12054 = CIRCLE ( 'NONE', #6972, 1.499999999999999556 ) ;
#12055 = EDGE_CURVE ( 'NONE', #6017, #8901, #13577, .T. ) ;
#12056 = CARTESIAN_POINT ( 'NONE',  ( -65.30644784966793281, -30.60858878180435738, 12.99038105676661736 ) ) ;
#12058 = DIRECTION ( 'NONE',  ( -0.9876526153536336894, -0.1566598588826349503, 0.000000000000000000 ) ) ;
#12057 = VECTOR ( 'NONE', #7047, 1000.000000000000000 ) ;
#12059 = CARTESIAN_POINT ( 'NONE',  ( -49.59961335071797350, 35.00051552679458666, -130.3485206753969976 ) ) ;
#12060 = AXIS2_PLACEMENT_3D ( 'NONE', #10463, #10827, #635 ) ;
#12061 = EDGE_LOOP ( 'NONE', ( #11925, #4858 ) ) ;
#12062 = LINE ( 'NONE', #6229, #11208 ) ;
#12063 = AXIS2_PLACEMENT_3D ( 'NONE', #163, #17528, #7461 ) ;
#12064 = TOROIDAL_SURFACE ( 'NONE', #14523, 3.000000000000000000, 2.000000000000000000 ) ;
#12065 = LINE ( 'NONE', #17044, #7285 ) ;
#12066 = EDGE_LOOP ( 'NONE', ( #16876, #15300, #2479, #15704 ) ) ;
#12067 = VERTEX_POINT ( 'NONE', #13125 ) ;
#12068 = EDGE_LOOP ( 'NONE', ( #8690, #16468, #15194, #2584 ) ) ;
#12069 = ORIENTED_EDGE ( 'NONE', *, *, #18375, .T. ) ;
#12070 = CIRCLE ( 'NONE', #916, 1.500000000000001332 ) ;
#12071 = AXIS2_PLACEMENT_3D ( 'NONE', #10539, #10356, #16152 ) ;
#12072 = LINE ( 'NONE', #5949, #7197 ) ;
#12073 = VERTEX_POINT ( 'NONE', #157 ) ;
#12074 = DIRECTION ( 'NONE',  ( -0.1566598588826321192, 0.9876526153536342445, 7.798540720466731404E-17 ) ) ;
#12075 = PLANE ( 'NONE',  #2225 ) ;
#12076 = AXIS2_PLACEMENT_3D ( 'NONE', #2525, #2612, #17238 ) ;
#12077 = EDGE_LOOP ( 'NONE', ( #15372, #5341, #13957, #11992 ) ) ;
#12078 = CARTESIAN_POINT ( 'NONE',  ( 0.000000000000000000, 0.000000000000000000, -25.00000000000000000 ) ) ;
#12079 = SURFACE_STYLE_FILL_AREA ( #16386 ) ;
#12080 = PRODUCT ( 'Heavy Presser Piston Block', 'Heavy Presser Piston Block', '', ( #6985 ) ) ;
#12081 = DIRECTION ( 'NONE',  ( -0.9876526153536341335, -0.1566598588826327021, 0.000000000000000000 ) ) ;
#12082 = CARTESIAN_POINT ( 'NONE',  ( -61.31620237807555895, -87.68113078262194904, -4.330127018922185655 ) ) ;
#12083 = DIRECTION ( 'NONE',  ( 0.000000000000000000, 0.000000000000000000, 1.000000000000000000 ) ) ;
#12084 = ORIENTED_EDGE ( 'NONE', *, *, #2633, .T. ) ;
#12085 = LINE ( 'NONE', #17935, #8488 ) ;
#12086 = EDGE_CURVE ( 'NONE', #11320, #8678, #8607, .T. ) ;
#12087 = AXIS2_PLACEMENT_3D ( 'NONE', #13902, #9652, #12485 ) ;
#12088 = DIRECTION ( 'NONE',  ( -0.9876526153536336894, -0.1566598588826349503, 0.000000000000000000 ) ) ;
#12090 = VERTEX_POINT ( 'NONE', #1670 ) ;
#12089 = DIRECTION ( 'NONE',  ( -0.1566598588826321192, 0.9876526153536342445, 7.798540720466730171E-17 ) ) ;
#12091 = CIRCLE ( 'NONE', #6993, 150.0000000000000284 ) ;
#12092 = LINE ( 'NONE', #3663, #4753 ) ;
#12093 = EDGE_LOOP ( 'NONE', ( #1747, #3976 ) ) ;
#12094 = AXIS2_PLACEMENT_3D ( 'NONE', #2878, #14172, #15679 ) ;
#12095 = EDGE_LOOP ( 'NONE', ( #4263, #35 ) ) ;
#12096 = ADVANCED_FACE ( 'NONE', ( #7284 ), #13035, .F. ) ;
#12097 = VERTEX_POINT ( 'NONE', #17342 ) ;
#12098 = EDGE_LOOP ( 'NONE', ( #64, #18719 ) ) ;
#12099 = CARTESIAN_POINT ( 'NONE',  ( -31.72625892764450839, -25.28215357979487266, 8.660254037844417496 ) ) ;
#12100 = ORIENTED_EDGE ( 'NONE', *, *, #18751, .T. ) ;
#12101 = AXIS2_PLACEMENT_3D ( 'NONE', #14462, #1490, #7276 ) ;
#12102 = LINE ( 'NONE', #11998, #7077 ) ;
#12103 = VECTOR ( 'NONE', #11119, 1000.000000000000000 ) ;
#12104 = DIRECTION ( 'NONE',  ( -0.9876526153536336894, -0.1566598588826350336, 0.000000000000000000 ) ) ;
#12105 = LINE ( 'NONE', #10611, #987 ) ;
#12106 = DIRECTION ( 'NONE',  ( -0.000000000000000000, -0.000000000000000000, -1.000000000000000000 ) ) ;
#12107 = CARTESIAN_POINT ( 'NONE',  ( -46.50141314777111745, -85.33123289938247069, -12.99038105676658539 ) ) ;
#12108 = DIRECTION ( 'NONE',  ( -0.9876526153536336894, -0.1566598588826349503, 0.000000000000000000 ) ) ;
#12109 = VERTEX_POINT ( 'NONE', #4503 ) ;
#12110 = VECTOR ( 'NONE', #6806, 1000.000000000000000 ) ;
#12111 = DIRECTION ( 'NONE',  ( 0.000000000000000000, 0.000000000000000000, 1.000000000000000000 ) ) ;
#12112 = ORIENTED_EDGE ( 'NONE', *, *, #12136, .F. ) ;
#12113 = ADVANCED_FACE ( 'NONE', ( #18692 ), #6030, .F. ) ;
#12114 = CARTESIAN_POINT ( 'NONE',  ( -69.99999999999998579, -45.00000000000000711, -25.00000000000000000 ) ) ;
#12115 = AXIS2_PLACEMENT_3D ( 'NONE', #5870, #8425, #17357 ) ;
#12116 = ORIENTED_EDGE ( 'NONE', *, *, #1524, .F. ) ;
#12117 = FACE_OUTER_BOUND ( 'NONE', #16520, .T. ) ;
#12118 = ORIENTED_EDGE ( 'NONE', *, *, #11997, .F. ) ;
#12119 = EDGE_CURVE ( 'NONE', #4650, #15970, #279, .T. ) ;
#12120 = ORIENTED_EDGE ( 'NONE', *, *, #10396, .F. ) ;
#12121 = EDGE_LOOP ( 'NONE', ( #17092, #404 ) ) ;
#12122 = CYLINDRICAL_SURFACE ( 'NONE', #4716, 1.500000000000001554 ) ;
#12123 = AXIS2_PLACEMENT_3D ( 'NONE', #8656, #14344, #12898 ) ;
#12124 = FACE_BOUND ( 'NONE', #857, .T. ) ;
#12125 = EDGE_LOOP ( 'NONE', ( #5706, #6104 ) ) ;
#12126 = AXIS2_PLACEMENT_3D ( 'NONE', #3754, #7955, #5097 ) ;
#12127 = AXIS2_PLACEMENT_3D ( 'NONE', #13655, #699, #14995 ) ;
#12128 = EDGE_CURVE ( 'NONE', #777, #14841, #18181, .T. ) ;
#12129 = FACE_BOUND ( 'NONE', #3126, .T. ) ;
#12130 = EDGE_LOOP ( 'NONE', ( #6383, #3834, #15939, #12147, #6143, #6412, #5554 ) ) ;
#12131 = CARTESIAN_POINT ( 'NONE',  ( 73.09088021254186174, 1.387778780781445676E-14, -19.99999999999999645 ) ) ;
#12132 = ORIENTED_EDGE ( 'NONE', *, *, #9371, .T. ) ;
#12133 = CARTESIAN_POINT ( 'NONE',  ( 5.481473465377026066, -12.88229205725314586, 20.00000000000000000 ) ) ;
#12134 = DIRECTION ( 'NONE',  ( -0.000000000000000000, -0.000000000000000000, -1.000000000000000000 ) ) ;
#12135 = AXIS2_PLACEMENT_3D ( 'NONE', #9273, #7683, #283 ) ;
#12136 = EDGE_CURVE ( 'NONE', #17252, #5489, #10374, .T. ) ;
#12137 = CYLINDRICAL_SURFACE ( 'NONE', #8028, 1.500000000000001554 ) ;
#12138 = EDGE_CURVE ( 'NONE', #16672, #12097, #5752, .T. ) ;
#12139 = VERTEX_POINT ( 'NONE', #17425 ) ;
#12140 = VERTEX_POINT ( 'NONE', #4410 ) ;
#12141 = CARTESIAN_POINT ( 'NONE',  ( -47.98289207080156871, -85.56622268770641426, -12.99038105676658539 ) ) ;
#12142 = EDGE_CURVE ( 'NONE', #14841, #3425, #17518, .T. ) ;
#12143 = ORIENTED_EDGE ( 'NONE', *, *, #8250, .F. ) ;
#12144 = EDGE_CURVE ( 'NONE', #15928, #11588, #4225, .T. ) ;
#12145 = DIRECTION ( 'NONE',  ( 2.887450008416415878E-16, 0.000000000000000000, 1.000000000000000000 ) ) ;
#12146 = COLOUR_RGB ( '', 0.66274510, 0.83137255, 0.94901961) ;
#12147 = ORIENTED_EDGE ( 'NONE', *, *, #17812, .F. ) ;
#12148 = EDGE_CURVE ( 'NONE', #9105, #3382, #3893, .T. ) ;
#12149 = EDGE_CURVE ( 'NONE', #3917, #2189, #7860, .T. ) ;
#12150 = EDGE_LOOP ( 'NONE', ( #17393, #14012, #9362, #17203 ) ) ;
#12151 = ORIENTED_EDGE ( 'NONE', *, *, #3556, .F. ) ;
#12152 = CYLINDRICAL_SURFACE ( 'NONE', #3963, 5.000000000000004441 ) ;
#12153 = ORIENTED_EDGE ( 'NONE', *, *, #5351, .F. ) ;
#12154 = CIRCLE ( 'NONE', #3982, 1.500000000000001332 ) ;
#12155 = CARTESIAN_POINT ( 'NONE',  ( -53.90880776292333820, -86.50618184100221697, -8.660254037844385522 ) ) ;
#12156 = CYLINDRICAL_SURFACE ( 'NONE', #4212, 1.500000000000001554 ) ;
#12157 = EDGE_LOOP ( 'NONE', ( #10498, #8574 ) ) ;
#12158 = DIRECTION ( 'NONE',  ( -0.1566598588826321747, 0.9876526153536343555, 0.000000000000000000 ) ) ;
#12159 = FACE_OUTER_BOUND ( 'NONE', #5423, .T. ) ;
#12160 = DIRECTION ( 'NONE',  ( -0.9876526153536336894, -0.1566598588826349503, 0.000000000000000000 ) ) ;
#12161 = EDGE_CURVE ( 'NONE', #795, #7723, #14825, .T. ) ;
#12162 = VERTEX_POINT ( 'NONE', #5051 ) ;
#12163 = EDGE_LOOP ( 'NONE', ( #573, #13493 ) ) ;
#12164 = DIRECTION ( 'NONE',  ( -0.9876526153536336894, -0.1566598588826349503, 0.000000000000000000 ) ) ;
#12165 = ORIENTED_EDGE ( 'NONE', *, *, #8786, .T. ) ;
#12166 = VERTEX_POINT ( 'NONE', #9235 ) ;
#12167 = EDGE_CURVE ( 'NONE', #3425, #11543, #13910, .T. ) ;
#12168 = DIRECTION ( 'NONE',  ( -0.1566598588826321192, 0.9876526153536342445, 7.798540720466730171E-17 ) ) ;
#12169 = PRODUCT_DEFINITION ( 'UNKNOWN', '', #8999, #10413 ) ;
#12170 = VERTEX_POINT ( 'NONE', #17996 ) ;
#12171 = EDGE_CURVE ( 'NONE', #2476, #10913, #17894, .T. ) ;
#12172 = ADVANCED_FACE ( 'NONE', ( #7921, #15017 ), #4955, .T. ) ;
#12173 = DIRECTION ( 'NONE',  ( 2.735665993912342121E-16, 0.000000000000000000, 1.000000000000000000 ) ) ;
#12174 = LINE ( 'NONE', #13605, #14830 ) ;
#12175 = VECTOR ( 'NONE', #14103, 1000.000000000000000 ) ;
#12176 = CARTESIAN_POINT ( 'NONE',  ( -3.000000000000000000, 0.000000000000000000, -35.00000000000000000 ) ) ;
#12177 = VERTEX_POINT ( 'NONE', #7824 ) ;
#12178 = CARTESIAN_POINT ( 'NONE',  ( -71.02801022084922522, -26.45362499944937795, -4.330127018922180326 ) ) ;
#12179 = DIRECTION ( 'NONE',  ( -0.1566598588826321747, 0.9876526153536343555, 0.000000000000000000 ) ) ;
#12180 = ORIENTED_EDGE ( 'NONE', *, *, #16472, .F. ) ;
#12181 = CARTESIAN_POINT ( 'NONE',  ( -35.67686938905902849, -25.90879301532540779, 21.65063509461101887 ) ) ;
#12182 = FACE_BOUND ( 'NONE', #16140, .T. ) ;
#12183 = DIRECTION ( 'NONE',  ( 0.000000000000000000, 0.000000000000000000, 1.000000000000000000 ) ) ;
#12184 = CARTESIAN_POINT ( 'NONE',  ( -34.19539046602857724, -25.67380322700145356, 4.330127018922217630 ) ) ;
#12185 = CYLINDRICAL_SURFACE ( 'NONE', #10879, 1.500000000000001554 ) ;
#12186 = DIRECTION ( 'NONE',  ( -0.9876526153536341335, -0.1566598588826327021, 0.000000000000000000 ) ) ;
#12188 = ORIENTED_EDGE ( 'NONE', *, *, #17096, .F. ) ;
#12187 = LINE ( 'NONE', #13794, #3880 ) ;
#12189 = CARTESIAN_POINT ( 'NONE',  ( -56.37793930130739994, -86.89783148820880854, 21.65063509461101532 ) ) ;
#12190 = AXIS2_PLACEMENT_3D ( 'NONE', #15613, #17160, #15825 ) ;
#12191 = ORIENTED_EDGE ( 'NONE', *, *, #17071, .T. ) ;
#12192 = ADVANCED_FACE ( 'NONE', ( #13679 ), #724, .F. ) ;
#12193 = ORIENTED_EDGE ( 'NONE', *, *, #14335, .F. ) ;
#12194 = DIRECTION ( 'NONE',  ( 0.000000000000000000, 0.000000000000000000, 1.000000000000000000 ) ) ;
#12195 = EDGE_CURVE ( 'NONE', #9141, #4403, #1227, .T. ) ;
#12196 = LINE ( 'NONE', #3476, #17984 ) ;
#12197 = ORIENTED_EDGE ( 'NONE', *, *, #15529, .T. ) ;
#12198 = CARTESIAN_POINT ( 'NONE',  ( 0.000000000000000000, 0.000000000000000000, -35.00000000000000000 ) ) ;
#12199 = DIRECTION ( 'NONE',  ( 0.1856185419698762884, -0.9826218788918641422, 0.000000000000000000 ) ) ;
#12200 = CYLINDRICAL_SURFACE ( 'NONE', #11056, 1.500000000000001554 ) ;
#12201 = DIRECTION ( 'NONE',  ( -0.9876526153536336894, -0.1566598588826349503, 0.000000000000000000 ) ) ;
#12202 = ORIENTED_EDGE ( 'NONE', *, *, #8696, .F. ) ;
#12204 = ORIENTED_EDGE ( 'NONE', *, *, #9229, .F. ) ;
#12203 = FACE_OUTER_BOUND ( 'NONE', #9320, .T. ) ;
#12205 = CARTESIAN_POINT ( 'NONE',  ( -62.63296299034339398, -25.12201619894700855, -4.330127018922180326 ) ) ;
#12206 = LINE ( 'NONE', #18144, #13891 ) ;
#12207 = ORIENTED_EDGE ( 'NONE', *, *, #17118, .F. ) ;
#12208 = VERTEX_POINT ( 'NONE', #13313 ) ;
#12209 = ORIENTED_EDGE ( 'NONE', *, *, #5945, .F. ) ;
#12210 = ORIENTED_EDGE ( 'NONE', *, *, #13759, .F. ) ;
#12211 = ORIENTED_EDGE ( 'NONE', *, *, #7255, .T. ) ;
#12212 = DIRECTION ( 'NONE',  ( -1.000000000000000000, 0.000000000000000000, 0.000000000000000000 ) ) ;
#12213 = EDGE_LOOP ( 'NONE', ( #11912, #3579, #13630, #11952 ) ) ;
#12214 = FACE_BOUND ( 'NONE', #17819, .T. ) ;
#12215 = ORIENTED_EDGE ( 'NONE', *, *, #8841, .T. ) ;
#12216 = EDGE_CURVE ( 'NONE', #14341, #1903, #6363, .T. ) ;
#12217 = CARTESIAN_POINT ( 'NONE',  ( -84.16561914167408531, 33.59999999999999432, -30.00000000000000000 ) ) ;
#12218 = AXIS2_PLACEMENT_3D ( 'NONE', #5577, #5111, #10886 ) ;
#12219 = ORIENTED_EDGE ( 'NONE', *, *, #8292, .F. ) ;
#12220 = DIRECTION ( 'NONE',  ( -0.1566598588826321192, 0.9876526153536342445, 7.798540720466731404E-17 ) ) ;
#12221 = EDGE_CURVE ( 'NONE', #7418, #12715, #9369, .T. ) ;
#12222 = FACE_BOUND ( 'NONE', #7587, .T. ) ;
#12223 = DIRECTION ( 'NONE',  ( -0.1566598588826321192, 0.9876526153536342445, 7.798540720466730171E-17 ) ) ;
#12224 = ORIENTED_EDGE ( 'NONE', *, *, #5448, .T. ) ;
#12225 = CARTESIAN_POINT ( 'NONE',  ( -4.361458684479201153, -15.87908452487173427, 8.660254037844412167 ) ) ;
#12226 = DIRECTION ( 'NONE',  ( -0.1566598588826321192, 0.9876526153536342445, 7.798540720466730171E-17 ) ) ;
#12227 = LINE ( 'NONE', #10805, #10743 ) ;
#12228 = ORIENTED_EDGE ( 'NONE', *, *, #17775, .F. ) ;
#12229 = ORIENTED_EDGE ( 'NONE', *, *, #13917, .T. ) ;
#12230 = DIRECTION ( 'NONE',  ( -0.9876526153536336894, -0.1566598588826349503, 0.000000000000000000 ) ) ;
#12231 = FACE_OUTER_BOUND ( 'NONE', #17858, .T. ) ;
#12232 = EDGE_LOOP ( 'NONE', ( #7599, #3172 ) ) ;
#12233 = FACE_OUTER_BOUND ( 'NONE', #988, .T. ) ;
#12234 = VERTEX_POINT ( 'NONE', #7546 ) ;
#12235 = CYLINDRICAL_SURFACE ( 'NONE', #16398, 1.500000000000000888 ) ;
#12236 = CARTESIAN_POINT ( 'NONE',  ( -174.4265963546509965, 55.91158385207030790, -3.719291248522901050 ) ) ;
#12237 = ORIENTED_EDGE ( 'NONE', *, *, #5725, .F. ) ;
#12238 = FACE_BOUND ( 'NONE', #18146, .T. ) ;
#12239 = EDGE_CURVE ( 'NONE', #9341, #5533, #4828, .T. ) ;
#12240 = CARTESIAN_POINT ( 'NONE',  ( -67.77557938805200877, -31.00023842901093118, -8.660254037844380193 ) ) ;
#12241 = ADVANCED_FACE ( 'NONE', ( #14837 ), #6223, .F. ) ;
#12242 = CIRCLE ( 'NONE', #477, 1.499999999999999556 ) ;
#12243 = DIRECTION ( 'NONE',  ( 0.000000000000000000, 0.000000000000000000, 1.000000000000000000 ) ) ;
#12244 = CARTESIAN_POINT ( 'NONE',  ( -72.57741747767370555, 46.09670278008585598, 3.004020071001521686 ) ) ;
#12245 = DIRECTION ( 'NONE',  ( 1.000000000000000000, 0.000000000000000000, 0.000000000000000000 ) ) ;
#12246 = EDGE_CURVE ( 'NONE', #14796, #62, #9, .T. ) ;
#12247 = CARTESIAN_POINT ( 'NONE',  ( -34.15575545585074480, -83.37298466334958391, -17.32050807568878525 ) ) ;
#12248 = LINE ( 'NONE', #18083, #15032 ) ;
#12249 = CARTESIAN_POINT ( 'NONE',  ( -14.40270314877813895, -80.23978748569695085, 1.424741226644455312E-14 ) ) ;
#12250 = LINE ( 'NONE', #5056, #464 ) ;
#12251 = DIRECTION ( 'NONE',  ( -0.9876526153536341335, -0.1566598588826327021, 0.000000000000000000 ) ) ;
#12252 = ORIENTED_EDGE ( 'NONE', *, *, #955, .F. ) ;
#12253 = VERTEX_POINT ( 'NONE', #10662 ) ;
#12254 = DIRECTION ( 'NONE',  ( -0.1566598588826321747, 0.9876526153536343555, 0.000000000000000000 ) ) ;
#12255 = AXIS2_PLACEMENT_3D ( 'NONE', #15796, #9299, #15078 ) ;
#12256 = VERTEX_POINT ( 'NONE', #15113 ) ;
#12257 = ORIENTED_EDGE ( 'NONE', *, *, #7737, .F. ) ;
#12258 = DIRECTION ( 'NONE',  ( -0.1566598588826321192, 0.9876526153536342445, 7.798540720466730171E-17 ) ) ;
#12259 = AXIS2_PLACEMENT_3D ( 'NONE', #2417, #8205, #13977 ) ;
#12260 = ORIENTED_EDGE ( 'NONE', *, *, #5217, .F. ) ;
#12261 = DIRECTION ( 'NONE',  ( -0.9876526153536341335, -0.1566598588826327021, 0.000000000000000000 ) ) ;
#12262 = FACE_OUTER_BOUND ( 'NONE', #7110, .T. ) ;
#12263 = DIRECTION ( 'NONE',  ( -0.1566598588826321192, 0.9876526153536342445, 7.798540720466731404E-17 ) ) ;
#12264 = EDGE_CURVE ( 'NONE', #5148, #8214, #16964, .T. ) ;
#12265 = ADVANCED_FACE ( 'NONE', ( #16540 ), #9330, .F. ) ;
#12266 = CARTESIAN_POINT ( 'NONE',  ( -24.11451099155181055, -19.01228170252437266, -8.660254037844380193 ) ) ;
#12267 = AXIS2_PLACEMENT_3D ( 'NONE', #14239, #14037, #7062 ) ;
#12268 = CARTESIAN_POINT ( 'NONE',  ( -2.000000000000000000, 0.000000000000000000, 35.00000000000000000 ) ) ;
#12269 = CARTESIAN_POINT ( 'NONE',  ( -49.79347899074616635, -23.08543803347281198, 21.65063509461101887 ) ) ;
#12270 = DIRECTION ( 'NONE',  ( 0.000000000000000000, 0.000000000000000000, 1.000000000000000000 ) ) ;
#12271 = AXIS2_PLACEMENT_3D ( 'NONE', #6838, #18441, #5406 ) ;
#12272 = LINE ( 'NONE', #12483, #6262 ) ;
#12273 = FACE_BOUND ( 'NONE', #385, .T. ) ;
#12274 = CARTESIAN_POINT ( 'NONE',  ( -19.17624791478365864, -18.22898240811121795, 17.32050807568881368 ) ) ;
#12275 = FACE_OUTER_BOUND ( 'NONE', #2275, .T. ) ;
#12277 = ORIENTED_EDGE ( 'NONE', *, *, #14813, .F. ) ;
#12276 = DIRECTION ( 'NONE',  ( -0.1566598588826321192, 0.9876526153536342445, 7.798540720466730171E-17 ) ) ;
#12278 = ORIENTED_EDGE ( 'NONE', *, *, #8506, .T. ) ;
#12279 = CARTESIAN_POINT ( 'NONE',  ( -20.16390053013728334, -18.38564226699385529, 12.99038105676661736 ) ) ;
#12280 = B_SPLINE_CURVE_WITH_KNOTS ( 'NONE', 3,
 ( #3036, #10510, #16304, #3391, #10971, #765, #17948, #16589, #6270, #12002, #10772, #9377, #9280, #18135, #10877, #3677 ),
 .UNSPECIFIED., .F., .F.,
 ( 4, 2, 2, 2, 2, 2, 2, 4 ),
 ( 0.000000000000000000, 0.0006035471611761549556, 0.001207094322352309911, 0.001810641483528464867, 0.002414188644704619822, 0.003017735805880774995, 0.003621282967056929734, 0.004828377289409239645 ),
 .UNSPECIFIED. ) ;
#12281 = CARTESIAN_POINT ( 'NONE',  ( -83.14047854185180597, 6.938893903907228378E-15, -24.99999999999999289 ) ) ;
#12282 = ORIENTED_EDGE ( 'NONE', *, *, #980, .T. ) ;
#12283 = VERTEX_POINT ( 'NONE', #815 ) ;
#12284 = DIRECTION ( 'NONE',  ( -0.1566598588826321747, 0.9876526153536343555, 0.000000000000000000 ) ) ;
#12285 = DIRECTION ( 'NONE',  ( 0.000000000000000000, 0.000000000000000000, -1.000000000000000000 ) ) ;
#12286 = ORIENTED_EDGE ( 'NONE', *, *, #17050, .T. ) ;
#12287 = CARTESIAN_POINT ( 'NONE',  ( -37.44782129882581501, -21.12718979743990033, -17.32050807568878170 ) ) ;
#12288 = FACE_OUTER_BOUND ( 'NONE', #15743, .T. ) ;
#12289 = CARTESIAN_POINT ( 'NONE',  ( -129.1237108893556353, 8.819507310261730737, -5.132104245558539724 ) ) ;
#12290 = CARTESIAN_POINT ( 'NONE',  ( -24.11451099155181055, -19.01228170252437977, 17.32050807568882078 ) ) ;
#12291 = CARTESIAN_POINT ( 'NONE',  ( 3.231158466157545206, -19.73726462726228092, 35.00000000000000000 ) ) ;
#12292 = CARTESIAN_POINT ( 'NONE',  ( -22.34355908178503469, -23.79388492040988012, 21.65063509461101177 ) ) ;
#12293 = DIRECTION ( 'NONE',  ( -0.1566598588826321192, 0.9876526153536342445, 7.798540720466731404E-17 ) ) ;
#12294 = CARTESIAN_POINT ( 'NONE',  ( -46.33669483700848701, -22.53712852738358308, -12.99038105676658006 ) ) ;
#12295 = EDGE_LOOP ( 'NONE', ( #13935, #4942 ) ) ;
#12296 = EDGE_CURVE ( 'NONE', #14180, #18619, #10579, .T. ) ;
#12297 = EDGE_CURVE ( 'NONE', #15938, #14768, #10868, .T. ) ;
#12298 = CARTESIAN_POINT ( 'NONE',  ( -30.73860631229088369, -25.12549372091224598, -4.330127018922181215 ) ) ;
#12299 = CARTESIAN_POINT ( 'NONE',  ( -94.14047854185179176, 6.938893903907228378E-15, -35.00000000000000000 ) ) ;
#12300 = VECTOR ( 'NONE', #10010, 1000.000000000000000 ) ;
#12301 = AXIS2_PLACEMENT_3D ( 'NONE', #12189, #5294, #3750 ) ;
#12302 = CARTESIAN_POINT ( 'NONE',  ( -64.31879523431430812, -30.45192892292171294, 17.32050807568881723 ) ) ;
#12303 = EDGE_CURVE ( 'NONE', #9105, #5608, #11829, .T. ) ;
#12304 = ORIENTED_EDGE ( 'NONE', *, *, #13940, .F. ) ;
#12305 = EDGE_LOOP ( 'NONE', ( #18544, #10042, #1895, #17106 ) ) ;
#12306 = EDGE_LOOP ( 'NONE', ( #14882, #2573, #6491, #15887 ) ) ;
#12307 = ORIENTED_EDGE ( 'NONE', *, *, #16350, .T. ) ;
#12308 = DIRECTION ( 'NONE',  ( -0.000000000000000000, -0.000000000000000000, -1.000000000000000000 ) ) ;
#12309 = AXIS2_PLACEMENT_3D ( 'NONE', #9995, #2807, #14365 ) ;
#12310 = FACE_BOUND ( 'NONE', #3732, .T. ) ;
#12311 = PRESENTATION_STYLE_ASSIGNMENT (( #6567 ) ) ;
#12312 = APPLICATION_CONTEXT ( 'automotive_design' ) ;
#12313 = ORIENTED_EDGE ( 'NONE', *, *, #17968, .F. ) ;
#12314 = DIRECTION ( 'NONE',  ( -0.1566598588826321192, 0.9876526153536342445, 7.798540720466730171E-17 ) ) ;
#12315 = ORIENTED_EDGE ( 'NONE', *, *, #10376, .F. ) ;
#12316 = DIRECTION ( 'NONE',  ( -0.1566598588826321192, 0.9876526153536342445, 7.798540720466730171E-17 ) ) ;
#12317 = ORIENTED_EDGE ( 'NONE', *, *, #11310, .T. ) ;
#12318 = DIRECTION ( 'NONE',  ( -0.1566598588826321192, 0.9876526153536342445, 7.798540720466730171E-17 ) ) ;
#12319 = LINE ( 'NONE', #1001, #10245 ) ;
#12320 = DIRECTION ( 'NONE',  ( -0.9876526153536336894, -0.1566598588826349503, 0.000000000000000000 ) ) ;
#12321 = CIRCLE ( 'NONE', #8461, 1.500000000000000888 ) ;
#12322 = EDGE_LOOP ( 'NONE', ( #7653, #8411 ) ) ;
#12323 = ORIENTED_EDGE ( 'NONE', *, *, #5216, .F. ) ;
#12324 = DIRECTION ( 'NONE',  ( -0.9876526153536336894, -0.1566598588826349503, 0.000000000000000000 ) ) ;
#12325 = ADVANCED_FACE ( 'NONE', ( #2311 ), #13972, .F. ) ;
#12326 = AXIS2_PLACEMENT_3D ( 'NONE', #9476, #5104, #3675 ) ;
#12327 = CARTESIAN_POINT ( 'NONE',  ( -169.3393727017007677, 31.92299471093763685, -3.150553392547038367 ) ) ;
#12328 = ORIENTED_EDGE ( 'NONE', *, *, #14034, .T. ) ;
#12329 = VERTEX_POINT ( 'NONE', #1105 ) ;
#12330 = DIRECTION ( 'NONE',  ( -0.1566598588826321192, 0.9876526153536342445, 7.798540720466730171E-17 ) ) ;
#12331 = CARTESIAN_POINT ( 'NONE',  ( -126.3445361634316981, -15.30092830501151369, 2.499999999999999556 ) ) ;
#12332 = EDGE_CURVE ( 'NONE', #15912, #13410, #17119, .T. ) ;
#12333 = ORIENTED_EDGE ( 'NONE', *, *, #8539, .T. ) ;
#12334 = VECTOR ( 'NONE', #1739, 1000.000000000000000 ) ;
#12335 = FACE_OUTER_BOUND ( 'NONE', #1174, .T. ) ;
#12336 = AXIS2_PLACEMENT_3D ( 'NONE', #18665, #5636, #11391 ) ;
#12337 = AXIS2_PLACEMENT_3D ( 'NONE', #12035, #17882, #7714 ) ;
#12338 = CARTESIAN_POINT ( 'NONE',  ( -71.14534172961498371, 45.48734807996677176, 4.189415517288649582 ) ) ;
#12339 = SURFACE_STYLE_FILL_AREA ( #18189 ) ;
#12340 = CIRCLE ( 'NONE', #10824, 1.500000000000000444 ) ;
#12341 = B_SPLINE_CURVE_WITH_KNOTS ( 'NONE', 3,
 ( #8700, #2740, #15611, #12949 ),
 .UNSPECIFIED., .F., .F.,
 ( 4, 4 ),
 ( 0.000000000000000000, 0.003000475340473846009 ),
 .UNSPECIFIED. ) ;
#12342 = FACE_OUTER_BOUND ( 'NONE', #13115, .T. ) ;
#12343 = PRESENTATION_STYLE_ASSIGNMENT (( #13768 ) ) ;
#12344 = DIRECTION ( 'NONE',  ( -0.9876526153536341335, -0.1566598588826327021, 0.000000000000000000 ) ) ;
#12345 = CIRCLE ( 'NONE', #6953, 2.500000000000002220 ) ;
#12346 = DIRECTION ( 'NONE',  ( 0.000000000000000000, 0.000000000000000000, 1.000000000000000000 ) ) ;
#12347 = ORIENTED_EDGE ( 'NONE', *, *, #16731, .F. ) ;
#12348 = ORIENTED_EDGE ( 'NONE', *, *, #10659, .T. ) ;
#12349 = CARTESIAN_POINT ( 'NONE',  ( 11.77009115809307715, -76.08830122530719109, -17.32050807568878525 ) ) ;
#12350 = EDGE_CURVE ( 'NONE', #5485, #384, #13767, .T. ) ;
#12351 = AXIS2_PLACEMENT_3D ( 'NONE', #7605, #16038, #11734 ) ;
#12352 = ORIENTED_EDGE ( 'NONE', *, *, #12610, .F. ) ;
#12353 = ORIENTED_EDGE ( 'NONE', *, *, #7078, .T. ) ;
#12354 = CIRCLE ( 'NONE', #12029, 5.000000000000000000 ) ;
#12355 = CARTESIAN_POINT ( 'NONE',  ( -43.04462899403342391, -84.78292339329327376, -12.99038105676658539 ) ) ;
#12356 = AXIS2_PLACEMENT_3D ( 'NONE', #8980, #13618, #378 ) ;
#12357 = ORIENTED_EDGE ( 'NONE', *, *, #14608, .F. ) ;
#12358 = EDGE_LOOP ( 'NONE', ( #8962, #2563 ) ) ;
#12359 = DIRECTION ( 'NONE',  ( -0.9876526153536336894, -0.1566598588826349503, 0.000000000000000000 ) ) ;
#12361 = EDGE_CURVE ( 'NONE', #17699, #8605, #18193, .T. ) ;
#12360 = DIRECTION ( 'NONE',  ( -0.9876526153536336894, -0.1566598588826349503, 0.000000000000000000 ) ) ;
#12362 = EDGE_CURVE ( 'NONE', #3308, #13600, #3599, .T. ) ;
#12363 = CARTESIAN_POINT ( 'NONE',  ( -56.21322099054479082, -24.10372711620989961, -12.99038105676658006 ) ) ;
#12364 = VERTEX_POINT ( 'NONE', #6699 ) ;
#12365 = VECTOR ( 'NONE', #5350, 1000.000000000000000 ) ;
#12366 = DIRECTION ( 'NONE',  ( -0.1566598588826321192, 0.9876526153536342445, 7.798540720466730171E-17 ) ) ;
#12367 = DIRECTION ( 'NONE',  ( -1.000000000000000000, 0.000000000000000000, 0.000000000000000000 ) ) ;
#12368 = CARTESIAN_POINT ( 'NONE',  ( -57.89905323451571206, -29.43363984018462176, 1.869203119972154228E-14 ) ) ;
#12369 = AXIS2_PLACEMENT_3D ( 'NONE', #15628, #1165, #18446 ) ;
#12370 = ORIENTED_EDGE ( 'NONE', *, *, #2362, .F. ) ;
#12371 = DIRECTION ( 'NONE',  ( -0.9876526153536336894, -0.1566598588826349503, 0.000000000000000000 ) ) ;
#12372 = AXIS2_PLACEMENT_3D ( 'NONE', #2034, #12051, #4776 ) ;
#12373 = DIRECTION ( 'NONE',  ( 0.000000000000000000, 0.000000000000000000, 1.000000000000000000 ) ) ;
#12374 = CIRCLE ( 'NONE', #3006, 1.500000000000000888 ) ;
#12375 = CIRCLE ( 'NONE', #4524, 1.500000000000000000 ) ;
#12376 = ADVANCED_FACE ( 'NONE', ( #12342 ), #3905, .F. ) ;
#12377 = DIRECTION ( 'NONE',  ( 0.000000000000000000, 0.000000000000000000, 1.000000000000000000 ) ) ;
#12378 = CYLINDRICAL_SURFACE ( 'NONE', #6602, 1.500000000000001554 ) ;
#12379 = EDGE_LOOP ( 'NONE', ( #7930, #1737, #18394, #1889 ) ) ;
#12380 = FACE_OUTER_BOUND ( 'NONE', #4071, .T. ) ;
#12381 = ADVANCED_FACE ( 'NONE', ( #6790 ), #12729, .F. ) ;
#12382 = CARTESIAN_POINT ( 'NONE',  ( -37.15834831208948685, -26.14378280364935137, -4.330127018922181215 ) ) ;
#12384 = ORIENTED_EDGE ( 'NONE', *, *, #9011, .T. ) ;
#12383 = DIRECTION ( 'NONE',  ( -0.1566598588826321192, 0.9876526153536342445, 7.798540720466731404E-17 ) ) ;
#12385 = AXIS2_PLACEMENT_3D ( 'NONE', #6891, #12629, #18490 ) ;
#12386 = ADVANCED_FACE ( 'NONE', ( #1204 ), #4004, .F. ) ;
#12387 = VECTOR ( 'NONE', #10002, 1000.000000000000000 ) ;
#12388 = DIRECTION ( 'NONE',  ( 0.000000000000000000, 0.000000000000000000, 1.000000000000000000 ) ) ;
#12389 = EDGE_CURVE ( 'NONE', #1477, #13575, #18292, .T. ) ;
#12390 = VERTEX_POINT ( 'NONE', #15393 ) ;
#12391 = EDGE_CURVE ( 'NONE', #9794, #13473, #2412, .T. ) ;
#12392 = ORIENTED_EDGE ( 'NONE', *, *, #9066, .T. ) ;
#12393 = EDGE_LOOP ( 'NONE', ( #11553, #14598, #11099, #12546 ) ) ;
#12394 = AXIS2_PLACEMENT_3D ( 'NONE', #17322, #15664, #11395 ) ;
#12395 = VECTOR ( 'NONE', #8497, 1000.000000000000000 ) ;
#12396 = DIRECTION ( 'NONE',  ( -0.1566598588826321192, 0.9876526153536342445, 7.798540720466730171E-17 ) ) ;
#12397 = DIRECTION ( 'NONE',  ( -0.1566598588826321192, 0.9876526153536342445, 7.798540720466730171E-17 ) ) ;
#12398 = DIRECTION ( 'NONE',  ( -1.000000000000000000, 0.000000000000000000, -0.000000000000000000 ) ) ;
#12399 = CARTESIAN_POINT ( 'NONE',  ( -4.361458684479201153, -15.87908452487173427, 17.32050807568881368 ) ) ;
#12400 = AXIS2_PLACEMENT_3D ( 'NONE', #3092, #14661, #10109 ) ;
#12401 = CARTESIAN_POINT ( 'NONE',  ( -81.73462711737164454, 33.01666666666666572, -30.00000000000000000 ) ) ;
#12402 = CARTESIAN_POINT ( 'NONE',  ( -172.7326993491721225, 43.83249341393818810, 9.951701414186830458E-16 ) ) ;
#12403 = CARTESIAN_POINT ( 'NONE',  ( -34.68921677370540380, -25.75213315644277046, -17.32050807568878170 ) ) ;
#12404 = ORIENTED_EDGE ( 'NONE', *, *, #12148, .F. ) ;
#12405 = AXIS2_PLACEMENT_3D ( 'NONE', #3983, #15269, #18270 ) ;
#12406 = DIRECTION ( 'NONE',  ( 1.000000000000000000, 0.000000000000000000, 0.000000000000000000 ) ) ;
#12407 = DIRECTION ( 'NONE',  ( 0.000000000000000000, 0.000000000000000000, 1.000000000000000000 ) ) ;
#12408 = VECTOR ( 'NONE', #6178, 1000.000000000000000 ) ;
#12409 = EDGE_LOOP ( 'NONE', ( #3687, #5409, #4943 ) ) ;
#12410 = EDGE_CURVE ( 'NONE', #113, #11250, #8481, .T. ) ;
#12411 = CARTESIAN_POINT ( 'NONE',  ( -77.40662104346073136, 32.93835651487657401, 35.00000000000000000 ) ) ;
#12412 = ORIENTED_EDGE ( 'NONE', *, *, #11151, .T. ) ;
#12413 = VERTEX_POINT ( 'NONE', #8201 ) ;
#12414 = AXIS2_PLACEMENT_3D ( 'NONE', #1315, #7100, #4022 ) ;
#12415 = ORIENTED_EDGE ( 'NONE', *, *, #18701, .T. ) ;
#12416 = CARTESIAN_POINT ( 'NONE',  ( -76.90911978745816668, 1.387778780781445676E-14, 25.00000000000000000 ) ) ;
#12417 = AXIS2_PLACEMENT_3D ( 'NONE', #10103, #4234, #10014 ) ;
#12418 = FACE_BOUND ( 'NONE', #15173, .T. ) ;
#12419 = ADVANCED_FACE ( 'NONE', ( #1023 ), #18584, .F. ) ;
#12420 = FILL_AREA_STYLE_COLOUR ( '', #16134 ) ;
#12421 = AXIS2_PLACEMENT_3D ( 'NONE', #17541, #3240, #10117 ) ;
#12422 = VECTOR ( 'NONE', #9901, 1000.000000000000000 ) ;
#12423 = DIRECTION ( 'NONE',  ( -0.1566598588826321192, 0.9876526153536342445, 7.798540720466731404E-17 ) ) ;
#12424 = CARTESIAN_POINT ( 'NONE',  ( -66.08974714408108753, -25.67032570503622324, 4.330127018922218518 ) ) ;
#12425 = EDGE_LOOP ( 'NONE', ( #14659, #645 ) ) ;
#12426 = AXIS2_PLACEMENT_3D ( 'NONE', #8336, #1336, #4249 ) ;
#12427 = LINE ( 'NONE', #8360, #4245 ) ;
#12429 = CARTESIAN_POINT ( 'NONE',  ( -54.73174206751433957, -23.86873732788595603, -12.99038105676658006 ) ) ;
#12428 = CIRCLE ( 'NONE', #18239, 1.500000000000001332 ) ;
#12430 = CARTESIAN_POINT ( 'NONE',  ( -312.1404785418517918, -2.850701963179326892, -15.88900348692940945 ) ) ;
#12431 = LINE ( 'NONE', #5334, #7150 ) ;
#12432 = ORIENTED_EDGE ( 'NONE', *, *, #17724, .T. ) ;
#12433 = ORIENTED_EDGE ( 'NONE', *, *, #4343, .F. ) ;
#12434 = CARTESIAN_POINT ( 'NONE',  ( -6.830590222863280658, -16.27073417207831696, -12.99038105676658006 ) ) ;
#12435 = AXIS2_PLACEMENT_3D ( 'NONE', #12817, #17206, #9972 ) ;
#12436 = CARTESIAN_POINT ( 'NONE',  ( -167.8744510809501378, 32.07610638047782459, -2.499999999999995559 ) ) ;
#12437 = AXIS2_PLACEMENT_3D ( 'NONE', #16527, #3521, #9318 ) ;
#12438 = VERTEX_POINT ( 'NONE', #8299 ) ;
#12439 = ORIENTED_EDGE ( 'NONE', *, *, #3416, .T. ) ;
#12440 = FACE_OUTER_BOUND ( 'NONE', #7509, .T. ) ;
#12441 = DIRECTION ( 'NONE',  ( -0.9876526153536336894, -0.1566598588826349503, 0.000000000000000000 ) ) ;
#12442 = EDGE_CURVE ( 'NONE', #17604, #13102, #3003, .T. ) ;
#12443 = VECTOR ( 'NONE', #8039, 1000.000000000000000 ) ;
#12444 = AXIS2_PLACEMENT_3D ( 'NONE', #8749, #14632, #217 ) ;
#12445 = DIRECTION ( 'NONE',  ( -0.9876526153536344665, -0.1566598588826304539, 0.000000000000000000 ) ) ;
#12446 = EDGE_LOOP ( 'NONE', ( #11251, #11739, #1144, #11225, #797, #9505 ) ) ;
#12447 = EDGE_CURVE ( 'NONE', #8907, #1459, #16031, .T. ) ;
#12448 = CARTESIAN_POINT ( 'NONE',  ( -14.93616446663280328, -22.61893597879013740, 1.869203119972154228E-14 ) ) ;
#12449 = AXIS2_PLACEMENT_3D ( 'NONE', #8147, #13915, #11062 ) ;
#12450 = EDGE_CURVE ( 'NONE', #8310, #15166, #14634, .T. ) ;
#12451 = LINE ( 'NONE', #5259, #5116 ) ;
#12452 = SHAPE_REPRESENTATION_RELATIONSHIP ( 'NONE' , 'NONE' ,  #15677, #1445 ) ;
#12453 = AXIS2_PLACEMENT_3D ( 'NONE', #1270, #7325, #12802 ) ;
#12454 = DIRECTION ( 'NONE',  ( -0.9876526153536336894, -0.1566598588826349503, 0.000000000000000000 ) ) ;
#12455 = CARTESIAN_POINT ( 'NONE',  ( 3.868870235264020963, -77.34158009636824715, -8.660254037844389075 ) ) ;
#12456 = CYLINDRICAL_SURFACE ( 'NONE', #12959, 1.500000000000000666 ) ;
#12457 = VECTOR ( 'NONE', #18555, 1000.000000000000227 ) ;
#12458 = DIRECTION ( 'NONE',  ( -0.1566598588826321192, 0.9876526153536342445, 7.798540720466731404E-17 ) ) ;
#12459 = ORIENTED_EDGE ( 'NONE', *, *, #11233, .F. ) ;
#12460 = VERTEX_POINT ( 'NONE', #11660 ) ;
#12461 = CARTESIAN_POINT ( 'NONE',  ( -60.32854976272193426, -87.52447092373932946, 8.660254037844412167 ) ) ;
#12462 = CARTESIAN_POINT ( 'NONE',  ( 3.000000000000000000, 0.000000000000000000, 35.00000000000000000 ) ) ;
#12463 = ORIENTED_EDGE ( 'NONE', *, *, #5223, .T. ) ;
#12464 = CIRCLE ( 'NONE', #12763, 13.99999999999999822 ) ;
#12465 = DIRECTION ( 'NONE',  ( -0.1566598588826321192, 0.9876526153536342445, 7.798540720466730171E-17 ) ) ;
#12466 = VERTEX_POINT ( 'NONE', #8751 ) ;
#12467 = ORIENTED_EDGE ( 'NONE', *, *, #11352, .F. ) ;
#12468 = ORIENTED_EDGE ( 'NONE', *, *, #3929, .F. ) ;
#12469 = DIRECTION ( 'NONE',  ( -0.1566598588826321747, 0.9876526153536343555, 0.000000000000000000 ) ) ;
#12470 = CARTESIAN_POINT ( 'NONE',  ( -36.62488699423479943, -83.76463431055617548, 21.65063509461101532 ) ) ;
#12471 = CARTESIAN_POINT ( 'NONE',  ( -59.38053215754616332, -29.66862962850856533, -8.660254037844380193 ) ) ;
#12472 = CARTESIAN_POINT ( 'NONE',  ( -10.98555400521827607, -21.99229654325962002, 4.330127018922214077 ) ) ;
#12473 = CARTESIAN_POINT ( 'NONE',  ( -44.85521591397804997, -22.30213873905963595, -21.65063509461098334 ) ) ;
#12474 = CARTESIAN_POINT ( 'NONE',  ( -44.07191661956489526, -27.24040181582777009, -21.65063509461098334 ) ) ;
#12475 = DIRECTION ( 'NONE',  ( -0.1566598588826321192, 0.9876526153536342445, 7.798540720466730171E-17 ) ) ;
#12476 = EDGE_CURVE ( 'NONE', #14720, #12880, #4520, .T. ) ;
#12477 = CARTESIAN_POINT ( 'NONE',  ( -85.13801595139511846, 33.83333333333333570, 100.5765140304660861 ) ) ;
#12478 = CYLINDRICAL_SURFACE ( 'NONE', #8853, 1.500000000000000666 ) ;
#12479 = CIRCLE ( 'NONE', #13685, 1.500000000000000888 ) ;
#12480 = DIRECTION ( 'NONE',  ( -0.9876526153536336894, -0.1566598588826349503, 0.000000000000000000 ) ) ;
#12481 = EDGE_LOOP ( 'NONE', ( #1652, #13320 ) ) ;
#12482 = AXIS2_PLACEMENT_3D ( 'NONE', #9878, #4381, #18570 ) ;
#12483 = CARTESIAN_POINT ( 'NONE',  ( -57.36559191666103175, -87.05449134709142811, 8.660254037844412167 ) ) ;
#12484 = EDGE_CURVE ( 'NONE', #4403, #17089, #13179, .T. ) ;
#12485 = DIRECTION ( 'NONE',  ( 0.000000000000000000, 0.000000000000000000, 1.000000000000000000 ) ) ;
#12486 = EDGE_CURVE ( 'NONE', #2560, #1541, #9071, .T. ) ;
#12487 = ORIENTED_EDGE ( 'NONE', *, *, #12303, .T. ) ;
#12488 = DIRECTION ( 'NONE',  ( -0.9876526153536344665, -0.1566598588826304539, 0.000000000000000000 ) ) ;
#12489 = EDGE_LOOP ( 'NONE', ( #18455, #13955, #9209, #10505 ) ) ;
#12490 = ORIENTED_EDGE ( 'NONE', *, *, #9898, .T. ) ;
#12491 = CARTESIAN_POINT ( 'NONE',  ( -24.11451099155181055, -19.01228170252437977, 17.32050807568882078 ) ) ;
#12492 = ORIENTED_EDGE ( 'NONE', *, *, #15138, .F. ) ;
#12493 = DIRECTION ( 'NONE',  ( -0.9876526153536341335, -0.1566598588826327021, 0.000000000000000000 ) ) ;
#12494 = DIRECTION ( 'NONE',  ( -1.000000000000000000, 0.000000000000000000, 0.000000000000000000 ) ) ;
#12495 = CARTESIAN_POINT ( 'NONE',  ( -28.26947477390680774, -24.73384407370567217, 8.660254037844417496 ) ) ;
#12496 = ADVANCED_FACE ( 'NONE', ( #7356 ), #3064, .F. ) ;
#12497 = EDGE_CURVE ( 'NONE', #15027, #10665, #17571, .T. ) ;
#12498 = CARTESIAN_POINT ( 'NONE',  ( -129.1404785418517918, -2.850701963179328668, 9.951701414186818625E-16 ) ) ;
#12499 = CARTESIAN_POINT ( 'NONE',  ( -126.1404785418517918, 9.595891400605989219, -2.500000000000000000 ) ) ;
#12500 = CARTESIAN_POINT ( 'NONE',  ( 5.350349158294472218, -77.10659030804430358, 1.077796531449093893E-14 ) ) ;
#12501 = EDGE_CURVE ( 'NONE', #15663, #16739, #14268, .T. ) ;
#12502 = CARTESIAN_POINT ( 'NONE',  ( -4.361458684479201153, -15.87908452487173427, 8.660254037844412167 ) ) ;
#12503 = CARTESIAN_POINT ( 'NONE',  ( -78.43540483600145308, -27.62857394106911002, -17.32050807568878170 ) ) ;
#12504 = AXIS2_PLACEMENT_3D ( 'NONE', #11969, #4522, #13140 ) ;
#12505 = CYLINDRICAL_SURFACE ( 'NONE', #8709, 1.500000000000001554 ) ;
#12506 = LINE ( 'NONE', #12411, #9680 ) ;
#12507 = EDGE_LOOP ( 'NONE', ( #1007, #4187, #5989, #16356 ) ) ;
#12508 = ORIENTED_EDGE ( 'NONE', *, *, #18557, .F. ) ;
#12509 = ORIENTED_EDGE ( 'NONE', *, *, #5567, .T. ) ;
#12510 = LINE ( 'NONE', #11078, #2616 ) ;
#12511 = FACE_BOUND ( 'NONE', #6459, .T. ) ;
#12512 = CIRCLE ( 'NONE', #4353, 1.500000000000000888 ) ;
#12513 = DIRECTION ( 'NONE',  ( -0.1566598588826321747, 0.9876526153536343555, 0.000000000000000000 ) ) ;
#12514 = DIRECTION ( 'NONE',  ( -6.505213034913026604E-17, -0.000000000000000000, 1.000000000000000000 ) ) ;
#12515 = EDGE_CURVE ( 'NONE', #241, #9690, #11489, .T. ) ;
#12516 = CARTESIAN_POINT ( 'NONE',  ( -2.000000000000000000, 0.000000000000000000, 35.00000000000000000 ) ) ;
#12517 = CARTESIAN_POINT ( 'NONE',  ( -49.50400600400986661, -28.10203103968224880, 1.869203119972154228E-14 ) ) ;
#12518 = DIRECTION ( 'NONE',  ( -0.9876526153536341335, -0.1566598588826327021, 0.000000000000000000 ) ) ;
#12519 = DIRECTION ( 'NONE',  ( -0.1566598588826321192, 0.9876526153536342445, 7.798540720466730171E-17 ) ) ;
#12520 = LINE ( 'NONE', #18362, #15686 ) ;
#12521 = FACE_OUTER_BOUND ( 'NONE', #7615, .T. ) ;
#12522 = EDGE_LOOP ( 'NONE', ( #5091, #10250 ) ) ;
#12523 = DIRECTION ( 'NONE',  ( -0.1566598588826321192, 0.9876526153536342445, 7.798540720466730171E-17 ) ) ;
#12524 = CARTESIAN_POINT ( 'NONE',  ( -170.3900270404893718, 32.17034444718320430, -4.582591203971097649 ) ) ;
#12525 = EDGE_LOOP ( 'NONE', ( #2424, #14119 ) ) ;
#12526 = VERTEX_POINT ( 'NONE', #1654 ) ;
#12527 = CARTESIAN_POINT ( 'NONE',  ( -64.20000000000000284, 2.694222958124180951E-16, -25.00000000000000000 ) ) ;
#12528 = CARTESIAN_POINT ( 'NONE',  ( -15.88418207180859021, -80.47477727402088021, -17.32050807568878525 ) ) ;
#12529 = CARTESIAN_POINT ( 'NONE',  ( -168.8245792648350516, 31.94895759036034377, 2.821239268406344536 ) ) ;
#12530 = ORIENTED_EDGE ( 'NONE', *, *, #5923, .T. ) ;
#12531 = DIRECTION ( 'NONE',  ( -0.1566598588826321192, 0.9876526153536342445, 7.798540720466731404E-17 ) ) ;
#12532 =( LENGTH_UNIT ( ) NAMED_UNIT ( * ) SI_UNIT ( .MILLI., .METRE. ) );
#12533 = ORIENTED_EDGE ( 'NONE', *, *, #11006, .F. ) ;
#12534 = DIRECTION ( 'NONE',  ( -0.1566598588826321192, 0.9876526153536342445, 7.798540720466730171E-17 ) ) ;
#12535 = AXIS2_PLACEMENT_3D ( 'NONE', #13446, #3400, #14789 ) ;
#12536 = DIRECTION ( 'NONE',  ( -0.1566598588826321192, 0.9876526153536342445, 7.798540720466730171E-17 ) ) ;
#12537 = EDGE_CURVE ( 'NONE', #12880, #14720, #15455, .T. ) ;
#12538 = DIRECTION ( 'NONE',  ( -0.9876526153536341335, -0.1566598588826327021, 0.000000000000000000 ) ) ;
#12539 = DIRECTION ( 'NONE',  ( 1.000000000000000000, 0.000000000000000000, 0.000000000000000000 ) ) ;
#12540 = ORIENTED_EDGE ( 'NONE', *, *, #12052, .T. ) ;
#12541 = EDGE_CURVE ( 'NONE', #4419, #11990, #5838, .T. ) ;
#12542 = ORIENTED_EDGE ( 'NONE', *, *, #8453, .T. ) ;
#12543 = DIRECTION ( 'NONE',  ( -0.1566598588826321192, 0.9876526153536342445, 7.798540720466731404E-17 ) ) ;
#12544 = ORIENTED_EDGE ( 'NONE', *, *, #12296, .T. ) ;
#12545 = EDGE_CURVE ( 'NONE', #6414, #10326, #17588, .T. ) ;
#12546 = ORIENTED_EDGE ( 'NONE', *, *, #9539, .F. ) ;
#12547 = ORIENTED_EDGE ( 'NONE', *, *, #5814, .F. ) ;
#12548 = DIRECTION ( 'NONE',  ( -0.1566598588826321747, 0.9876526153536343555, 0.000000000000000000 ) ) ;
#12549 = AXIS2_PLACEMENT_3D ( 'NONE', #7455, #10377, #13216 ) ;
#12550 = DIRECTION ( 'NONE',  ( -0.1566598588826321747, 0.9876526153536343555, 0.000000000000000000 ) ) ;
#12551 = VERTEX_POINT ( 'NONE', #4203 ) ;
#12552 = CARTESIAN_POINT ( 'NONE',  ( -76.95392591297100182, -27.39358415274518066, 17.32050807568881723 ) ) ;
#12553 = DIRECTION ( 'NONE',  ( -0.1566598588826321192, 0.9876526153536342445, 7.798540720466730171E-17 ) ) ;
#12554 = CARTESIAN_POINT ( 'NONE',  ( -29.21749237908258223, -82.58968536893642920, 8.660254037844412167 ) ) ;
#12555 = FACE_OUTER_BOUND ( 'NONE', #1260, .T. ) ;
#12556 = EDGE_LOOP ( 'NONE', ( #17613, #18456 ) ) ;
#12557 = CARTESIAN_POINT ( 'NONE',  ( -53.74408945216069355, -23.71207746900333291, 17.32050807568882078 ) ) ;
#12558 = EDGE_LOOP ( 'NONE', ( #11839, #7362 ) ) ;
#12559 = DIRECTION ( 'NONE',  ( -0.1566598588826321192, 0.9876526153536342445, 7.798540720466730171E-17 ) ) ;
#12560 = ORIENTED_EDGE ( 'NONE', *, *, #18408, .T. ) ;
#12561 = CARTESIAN_POINT ( 'NONE',  ( -77.40662104346073136, 32.93835651487657401, -30.00000000000000000 ) ) ;
#12562 = AXIS2_PLACEMENT_3D ( 'NONE', #703, #7715, #17784 ) ;
#12563 = CARTESIAN_POINT ( 'NONE',  ( 2.000000000000000000, 2.449293598294706414E-16, -24.99999999999999289 ) ) ;
#12564 = ORIENTED_EDGE ( 'NONE', *, *, #15569, .F. ) ;
#12565 = EDGE_LOOP ( 'NONE', ( #16436, #14506 ) ) ;
#12566 = ADVANCED_FACE ( 'NONE', ( #9986 ), #15781, .F. ) ;
#12567 = DIRECTION ( 'NONE',  ( -0.1566598588826321747, 0.9876526153536343555, 0.000000000000000000 ) ) ;
#12568 = ORIENTED_EDGE ( 'NONE', *, *, #8503, .F. ) ;
#12569 = ORIENTED_EDGE ( 'NONE', *, *, #10175, .F. ) ;
#12570 = AXIS2_PLACEMENT_3D ( 'NONE', #12828, #17220, #1385 ) ;
#12571 = CARTESIAN_POINT ( 'NONE',  ( -74.62210677719829732, 46.96672731380024146, 2.500000000000000000 ) ) ;
#12572 = EDGE_CURVE ( 'NONE', #14170, #15556, #10284, .T. ) ;
#12573 = VERTEX_POINT ( 'NONE', #14715 ) ;
#12574 = DIRECTION ( 'NONE',  ( -0.1566598588826321192, 0.9876526153536342445, 7.798540720466731404E-17 ) ) ;
#12575 = VECTOR ( 'NONE', #11439, 1000.000000000000000 ) ;
#12576 = CARTESIAN_POINT ( 'NONE',  ( -28.22983976372896109, -82.43302551005379541, -4.330127018922185655 ) ) ;
#12577 = CARTESIAN_POINT ( 'NONE',  ( -43.08426400421124924, -27.08374195694514341, 1.869203119972154228E-14 ) ) ;
#12578 = LINE ( 'NONE', #18439, #2686 ) ;
#12579 = DIRECTION ( 'NONE',  ( -0.9876526153536341335, -0.1566598588826327021, 0.000000000000000000 ) ) ;
#12580 = EDGE_LOOP ( 'NONE', ( #8757, #2448, #1642, #16975 ) ) ;
#12581 = DIRECTION ( 'NONE',  ( -0.9876526153536336894, -0.1566598588826350336, 0.000000000000000000 ) ) ;
#12582 = CARTESIAN_POINT ( 'NONE',  ( -129.1404785418517918, -2.850701963179328668, 9.951701414186818625E-16 ) ) ;
#12583 = CIRCLE ( 'NONE', #9574, 1.500000000000001332 ) ;
#12584 = ORIENTED_EDGE ( 'NONE', *, *, #12839, .F. ) ;
#12585 = CYLINDRICAL_SURFACE ( 'NONE', #12369, 2.200000000000000622 ) ;
#12586 = EDGE_CURVE ( 'NONE', #14892, #5886, #16236, .T. ) ;
#12587 = CIRCLE ( 'NONE', #8968, 1.500000000000001332 ) ;
#12588 = ORIENTED_EDGE ( 'NONE', *, *, #909, .T. ) ;
#12589 = FACE_OUTER_BOUND ( 'NONE', #7394, .T. ) ;
#12590 = EDGE_CURVE ( 'NONE', #14949, #18590, #7712, .T. ) ;
#12591 = ORIENTED_EDGE ( 'NONE', *, *, #13563, .F. ) ;
#12592 = ORIENTED_EDGE ( 'NONE', *, *, #12450, .T. ) ;
#12593 = FACE_BOUND ( 'NONE', #3426, .T. ) ;
#12594 = EDGE_CURVE ( 'NONE', #9193, #13266, #9305, .T. ) ;
#12595 = VECTOR ( 'NONE', #17366, 1000.000000000000000 ) ;
#12596 = AXIS2_PLACEMENT_3D ( 'NONE', #18642, #9948, #14870 ) ;
#12597 = FILL_AREA_STYLE ('',( #12420 ) ) ;
#12598 = ORIENTED_EDGE ( 'NONE', *, *, #5945, .T. ) ;
#12599 = CIRCLE ( 'NONE', #15640, 1.500000000000001332 ) ;
#12600 = DIRECTION ( 'NONE',  ( 0.000000000000000000, 0.000000000000000000, 1.000000000000000000 ) ) ;
#12601 = EDGE_LOOP ( 'NONE', ( #10615, #1998 ) ) ;
#12602 = AXIS2_PLACEMENT_3D ( 'NONE', #16875, #18326, #5205 ) ;
#12603 = DIRECTION ( 'NONE',  ( -0.1566598588826321192, 0.9876526153536342445, 7.798540720466730171E-17 ) ) ;
#12604 = FACE_OUTER_BOUND ( 'NONE', #2919, .T. ) ;
#12605 = AXIS2_PLACEMENT_3D ( 'NONE', #12363, #12263, #7838 ) ;
#12606 = CARTESIAN_POINT ( 'NONE',  ( -37.15834831208949396, -26.14378280364935137, -21.65063509461098334 ) ) ;
#12607 = AXIS2_PLACEMENT_3D ( 'NONE', #6728, #5484, #8323 ) ;
#12608 = CYLINDRICAL_SURFACE ( 'NONE', #14187, 1.500000000000001554 ) ;
#12609 = EDGE_LOOP ( 'NONE', ( #15306, #8146, #10336, #9968 ) ) ;
#12610 = EDGE_CURVE ( 'NONE', #5860, #7782, #17972, .T. ) ;
#12611 = CARTESIAN_POINT ( 'NONE',  ( -58.88670584986932255, -29.59029969906724133, 21.65063509461101887 ) ) ;
#12612 = ORIENTED_EDGE ( 'NONE', *, *, #16728, .F. ) ;
#12613 = EDGE_LOOP ( 'NONE', ( #4232, #6429, #8961, #16556 ) ) ;
#12614 = CARTESIAN_POINT ( 'NONE',  ( -129.1404785418517918, -14.35070196317933444, 5.500000000000000000 ) ) ;
#12615 = EDGE_CURVE ( 'NONE', #12954, #14743, #18524, .T. ) ;
#12616 = ADVANCED_FACE ( 'NONE', ( #611 ), #14834, .T. ) ;
#12617 = EDGE_LOOP ( 'NONE', ( #3360, #17726, #15543, #16466 ) ) ;
#12618 = CARTESIAN_POINT ( 'NONE',  ( -127.6813802953510333, -15.23413708567786706, 2.918139657044713342 ) ) ;
#12619 = CIRCLE ( 'NONE', #7498, 1.499999999999999556 ) ;
#12620 = DIRECTION ( 'NONE',  ( 1.000000000000000000, 0.000000000000000000, -0.000000000000000000 ) ) ;
#12621 = ITEM_DEFINED_TRANSFORMATION ( 'NONE', 'NONE', #14750,  #18772 ) ;
#12622 = DIRECTION ( 'NONE',  ( -0.1566598588826321192, 0.9876526153536342445, 7.798540720466730171E-17 ) ) ;
#12623 = DIRECTION ( 'NONE',  ( -0.1566598588826321192, 0.9876526153536342445, 7.798540720466730171E-17 ) ) ;
#12624 = AXIS2_PLACEMENT_3D ( 'NONE', #15721, #10119, #5954 ) ;
#12625 = LINE ( 'NONE', #6793, #4480 ) ;
#12626 = DIRECTION ( 'NONE',  ( -0.1566598588826321192, 0.9876526153536342445, 7.798540720466731404E-17 ) ) ;
#12627 = ORIENTED_EDGE ( 'NONE', *, *, #8104, .F. ) ;
#12628 = ORIENTED_EDGE ( 'NONE', *, *, #1191, .F. ) ;
#12629 = DIRECTION ( 'NONE',  ( -0.1566598588826321192, 0.9876526153536342445, 7.798540720466731404E-17 ) ) ;
#12630 = DIRECTION ( 'NONE',  ( 0.000000000000000000, 0.000000000000000000, 1.000000000000000000 ) ) ;
#12631 = EDGE_LOOP ( 'NONE', ( #5327, #2291, #9473, #16767 ) ) ;
#12632 = ORIENTED_EDGE ( 'NONE', *, *, #13759, .T. ) ;
#12633 = VERTEX_POINT ( 'NONE', #3329 ) ;
#12634 = AXIS2_PLACEMENT_3D ( 'NONE', #4587, #10721, #9223 ) ;
#12635 = ORIENTED_EDGE ( 'NONE', *, *, #11852, .T. ) ;
#12636 = DIRECTION ( 'NONE',  ( -0.1566598588826321192, 0.9876526153536342445, 7.798540720466730171E-17 ) ) ;
#12637 = CIRCLE ( 'NONE', #14778, 2.000000000000001776 ) ;
#12638 = AXIS2_PLACEMENT_3D ( 'NONE', #3966, #3769, #682 ) ;
#12639 = DIRECTION ( 'NONE',  ( 0.000000000000000000, 0.000000000000000000, 1.000000000000000000 ) ) ;
#12640 = ADVANCED_FACE ( 'NONE', ( #4934 ), #17780, .F. ) ;
#12641 = CIRCLE ( 'NONE', #15688, 1.500000000000000888 ) ;
#12642 = VERTEX_POINT ( 'NONE', #13464 ) ;
#12643 = DIRECTION ( 'NONE',  ( -0.1566598588826321192, 0.9876526153536342445, 7.798540720466731404E-17 ) ) ;
#12644 = ADVANCED_FACE ( 'NONE', ( #18059 ), #1924, .F. ) ;
#12645 = CARTESIAN_POINT ( 'NONE',  ( -14.40270314877813895, -80.23978748569695085, 17.32050807568881368 ) ) ;
#12646 = PLANE ( 'NONE',  #10004 ) ;
#12647 = CARTESIAN_POINT ( 'NONE',  ( -26.74836084069850983, -82.19803572172985184, 21.65063509461101532 ) ) ;
#12648 = DIRECTION ( 'NONE',  ( -0.000000000000000000, -0.000000000000000000, -1.000000000000000000 ) ) ;
#12649 = ORIENTED_EDGE ( 'NONE', *, *, #17635, .T. ) ;
#12651 = DIRECTION ( 'NONE',  ( 0.000000000000000000, 0.000000000000000000, 1.000000000000000000 ) ) ;
#12650 = VECTOR ( 'NONE', #11400, 1000.000000000000000 ) ;
#12652 = AXIS2_PLACEMENT_3D ( 'NONE', #2746, #18628, #5597 ) ;
#12653 = LINE ( 'NONE', #5668, #13542 ) ;
#12654 = ORIENTED_EDGE ( 'NONE', *, *, #3481, .F. ) ;
#12655 = DIRECTION ( 'NONE',  ( -0.1566598588826321192, 0.9876526153536342445, 7.798540720466730171E-17 ) ) ;
#12657 = ORIENTED_EDGE ( 'NONE', *, *, #14128, .T. ) ;
#12656 = CYLINDRICAL_SURFACE ( 'NONE', #6963, 1.500000000000001554 ) ;
#12658 = CARTESIAN_POINT ( 'NONE',  ( 55.85952145814821534, 6.938893903907228378E-15, 100.5765140304660861 ) ) ;
#12659 = ORIENTED_EDGE ( 'NONE', *, *, #6025, .F. ) ;
#12660 = CLOSED_SHELL ( 'NONE', ( #13944, #10133, #9248, #7711, #2431, #5268, #13994, #16576, #4695, #13886 ) ) ;
#12661 = AXIS2_PLACEMENT_3D ( 'NONE', #18365, #3707, #10807 ) ;
#12662 = CARTESIAN_POINT ( 'NONE',  ( -27.73601345605213098, -82.35469558061248563, 17.32050807568881368 ) ) ;
#12663 = EDGE_CURVE ( 'NONE', #1265, #12921, #506, .T. ) ;
#12664 = LINE ( 'NONE', #2741, #17009 ) ;
#12665 = CIRCLE ( 'NONE', #4510, 1.500000000000000888 ) ;
#12666 = CARTESIAN_POINT ( 'NONE',  ( -2.000000000000000000, 0.000000000000000000, -35.00000000000000000 ) ) ;
#12667 = AXIS2_PLACEMENT_3D ( 'NONE', #6531, #14472, #4332 ) ;
#12668 = ORIENTED_EDGE ( 'NONE', *, *, #2193, .T. ) ;
#12669 = CYLINDRICAL_SURFACE ( 'NONE', #5519, 1.500000000000000666 ) ;
#12670 = LINE ( 'NONE', #5307, #2049 ) ;
#12671 = EDGE_CURVE ( 'NONE', #6385, #1601, #16335, .T. ) ;
#12672 = PLANE ( 'NONE',  #5415 ) ;
#12673 = DIRECTION ( 'NONE',  ( -0.9876526153536336894, -0.1566598588826350336, 0.000000000000000000 ) ) ;
#12674 = CYLINDRICAL_SURFACE ( 'NONE', #7748, 1.500000000000001554 ) ;
#12675 = AXIS2_PLACEMENT_3D ( 'NONE', #17587, #10345, #16047 ) ;
#12676 = FACE_OUTER_BOUND ( 'NONE', #3516, .T. ) ;
#12677 = DIRECTION ( 'NONE',  ( -0.9998476951563911586, 0.000000000000000000, 0.01745240643728354635 ) ) ;
#12678 = AXIS2_PLACEMENT_3D ( 'NONE', #15834, #9943, #11168 ) ;
#12679 = ADVANCED_FACE ( 'NONE', ( #10714 ), #6300, .F. ) ;
#12680 = AXIS2_PLACEMENT_3D ( 'NONE', #2597, #6988, #5550 ) ;
#12681 = VERTEX_POINT ( 'NONE', #4851 ) ;
#12682 = APPLICATION_CONTEXT ( 'automotive_design' ) ;
#12683 = FACE_OUTER_BOUND ( 'NONE', #11057, .T. ) ;
#12684 = LINE ( 'NONE', #17088, #7544 ) ;
#12685 = AXIS2_PLACEMENT_3D ( 'NONE', #2649, #10124, #8440 ) ;
#12686 = AXIS2_PLACEMENT_3D ( 'NONE', #15758, #1451, #10145 ) ;
#12687 = ORIENTED_EDGE ( 'NONE', *, *, #15067, .T. ) ;
#12688 = ORIENTED_EDGE ( 'NONE', *, *, #12138, .T. ) ;
#12689 = CARTESIAN_POINT ( 'NONE',  ( 0.000000000000000000, 0.000000000000000000, 30.00000000000000000 ) ) ;
#12690 = CARTESIAN_POINT ( 'NONE',  ( 2.349859322727720023, -14.81454612788783898, -1.559688948638727718E-15 ) ) ;
#12691 = CIRCLE ( 'NONE', #6986, 12.83663829214476948 ) ;
#12692 = LINE ( 'NONE', #7977, #8661 ) ;
#12693 = CARTESIAN_POINT ( 'NONE',  ( 5.000000000000000000, 0.000000000000000000, 30.00000000000000000 ) ) ;
#12694 = CIRCLE ( 'NONE', #13002, 1.500000000000000444 ) ;
#12695 = ORIENTED_EDGE ( 'NONE', *, *, #738, .F. ) ;
#12696 = VECTOR ( 'NONE', #7521, 1000.000000000000000 ) ;
#12697 = EDGE_CURVE ( 'NONE', #2990, #8283, #9027, .T. ) ;
#12698 = AXIS2_PLACEMENT_3D ( 'NONE', #12107, #3575, #13717 ) ;
#12699 = CARTESIAN_POINT ( 'NONE',  ( -37.15834831208948685, -26.14378280364935137, 21.65063509461101887 ) ) ;
#12700 = LINE ( 'NONE', #1084, #12457 ) ;
#12701 = EDGE_LOOP ( 'NONE', ( #624, #6202 ) ) ;
#12702 = DIRECTION ( 'NONE',  ( -0.9876526153536341335, -0.1566598588826327021, 0.000000000000000000 ) ) ;
#12703 = CYLINDRICAL_SURFACE ( 'NONE', #11789, 3.000000000000000000 ) ;
#12705 = EDGE_CURVE ( 'NONE', #16637, #14520, #3021, .T. ) ;
#12704 = CARTESIAN_POINT ( 'NONE',  ( -9.997901389864651378, -21.83563668437698269, -17.32050807568878170 ) ) ;
#12706 = AXIS2_PLACEMENT_3D ( 'NONE', #15315, #15134, #2153 ) ;
#12707 = ORIENTED_EDGE ( 'NONE', *, *, #5337, .F. ) ;
#12708 = DIRECTION ( 'NONE',  ( -0.1566598588826321192, 0.9876526153536342445, 7.798540720466730171E-17 ) ) ;
#12709 = CIRCLE ( 'NONE', #5470, 1.500000000000000888 ) ;
#12710 = VERTEX_POINT ( 'NONE', #11857 ) ;
#12711 = ORIENTED_EDGE ( 'NONE', *, *, #12671, .T. ) ;
#12712 = ORIENTED_EDGE ( 'NONE', *, *, #2238, .T. ) ;
#12713 = AXIS2_PLACEMENT_3D ( 'NONE', #16033, #11283, #5715 ) ;
#12714 = DIRECTION ( 'NONE',  ( -0.9876526153536336894, -0.1566598588826349503, 0.000000000000000000 ) ) ;
#12715 = VERTEX_POINT ( 'NONE', #17694 ) ;
#12716 = CIRCLE ( 'NONE', #9087, 3.000000000000000000 ) ;
#12717 = DIRECTION ( 'NONE',  ( 0.9201637183752249260, 0.3915338189555018777, -2.458192809297183803E-16 ) ) ;
#12718 = VECTOR ( 'NONE', #17135, 1000.000000000000000 ) ;
#12719 = DIRECTION ( 'NONE',  ( -0.1566598588826321192, 0.9876526153536342445, 7.798540720466730171E-17 ) ) ;
#12720 = EDGE_LOOP ( 'NONE', ( #11075, #11918, #1122, #12237 ) ) ;
#12721 = DIRECTION ( 'NONE',  ( -0.1566598588826321192, 0.9876526153536342445, 7.798540720466730171E-17 ) ) ;
#12722 = LINE ( 'NONE', #4090, #14232 ) ;
#12723 = CIRCLE ( 'NONE', #12414, 1.500000000000000888 ) ;
#12724 = AXIS2_PLACEMENT_3D ( 'NONE', #249, #6037, #8520 ) ;
#12725 = DIRECTION ( 'NONE',  ( -0.1566598588826321192, 0.9876526153536342445, 7.798540720466731404E-17 ) ) ;
#12726 = APPLICATION_PROTOCOL_DEFINITION ( 'draft international standard', 'automotive_design', 1998, #13300 ) ;
#12727 = EDGE_CURVE ( 'NONE', #10500, #10528, #16439, .T. ) ;
#12728 = EDGE_CURVE ( 'NONE', #17816, #8900, #6688, .T. ) ;
#12729 = CYLINDRICAL_SURFACE ( 'NONE', #7283, 1.500000000000001554 ) ;
#12730 = CYLINDRICAL_SURFACE ( 'NONE', #9381, 1.500000000000001554 ) ;
#12732 = ADVANCED_FACE ( 'NONE', ( #7625 ), #13383, .F. ) ;
#12731 = FACE_OUTER_BOUND ( 'NONE', #6384, .T. ) ;
#12733 = VECTOR ( 'NONE', #12717, 1000.000000000000114 ) ;
#12734 = DIRECTION ( 'NONE',  ( 0.1856185419698760941, -0.9826218788918640312, 0.000000000000000000 ) ) ;
#12735 = ORIENTED_EDGE ( 'NONE', *, *, #17754, .T. ) ;
#12736 = ORIENTED_EDGE ( 'NONE', *, *, #15864, .T. ) ;
#12737 = CARTESIAN_POINT ( 'NONE',  ( -55.39028668595377525, -86.74117162932617475, 17.32050807568881368 ) ) ;
#12738 = CARTESIAN_POINT ( 'NONE',  ( -57.85941822433786541, -87.13282127653273790, 4.330127018922213189 ) ) ;
#12739 = ADVANCED_FACE ( 'NONE', ( #17011 ), #15366, .F. ) ;
#12740 = LINE ( 'NONE', #10453, #6381 ) ;
#12741 = EDGE_CURVE ( 'NONE', #13951, #11811, #10902, .T. ) ;
#12742 = VECTOR ( 'NONE', #4194, 1000.000000000000000 ) ;
#12743 = CARTESIAN_POINT ( 'NONE',  ( -68.55887868246516348, -26.06197535224279349, -17.32050807568878170 ) ) ;
#12744 = ORIENTED_EDGE ( 'NONE', *, *, #10445, .F. ) ;
#12745 = LINE ( 'NONE', #3733, #5496 ) ;
#12746 = AXIS2_PLACEMENT_3D ( 'NONE', #2078, #16302, #7768 ) ;
#12747 = CARTESIAN_POINT ( 'NONE',  ( -30.20514499443620338, -82.74634522781904877, 21.65063509461101532 ) ) ;
#12748 = AXIS2_PLACEMENT_3D ( 'NONE', #5972, #1707, #8992 ) ;
#12749 = ORIENTED_EDGE ( 'NONE', *, *, #1298, .F. ) ;
#12750 = CARTESIAN_POINT ( 'NONE',  ( -69.99999999999998579, -45.00000000000000711, 110.7545852194966045 ) ) ;
#12751 = FACE_OUTER_BOUND ( 'NONE', #7934, .T. ) ;
#12752 = DIRECTION ( 'NONE',  ( 0.000000000000000000, 0.000000000000000000, 1.000000000000000000 ) ) ;
#12753 = PRESENTATION_STYLE_ASSIGNMENT (( #8404 ) ) ;
#12754 = EDGE_CURVE ( 'NONE', #9877, #4040, #9990, .T. ) ;
#12755 = CIRCLE ( 'NONE', #15806, 1.499999999999999556 ) ;
#12756 = EDGE_CURVE ( 'NONE', #16064, #9762, #17904, .T. ) ;
#12757 = DIRECTION ( 'NONE',  ( 1.000000000000000000, 0.000000000000000000, 0.000000000000000000 ) ) ;
#12758 = ORIENTED_EDGE ( 'NONE', *, *, #878, .T. ) ;
#12759 = CARTESIAN_POINT ( 'NONE',  ( -37.44782129882580080, -21.12718979743990388, -8.660254037844380193 ) ) ;
#12760 = DIRECTION ( 'NONE',  ( -0.1566598588826321747, 0.9876526153536343555, 0.000000000000000000 ) ) ;
#12761 = DIRECTION ( 'NONE',  ( 3.816390434826605238E-17, 0.000000000000000000, -1.000000000000000000 ) ) ;
#12762 = ORIENTED_EDGE ( 'NONE', *, *, #145, .F. ) ;
#12763 = AXIS2_PLACEMENT_3D ( 'NONE', #4702, #7669, #2156 ) ;
#12764 = CARTESIAN_POINT ( 'NONE',  ( -23.29157668696081629, -81.64972621564065491, 21.65063509461101532 ) ) ;
#12765 = PRODUCT_DEFINITION ( 'UNKNOWN', '', #8096, #4091 ) ;
#12766 = CARTESIAN_POINT ( 'NONE',  ( -79.91688375903190433, -27.86356372939306070, -8.660254037844380193 ) ) ;
#12768 = EDGE_LOOP ( 'NONE', ( #15401, #542 ) ) ;
#12767 = CYLINDRICAL_SURFACE ( 'NONE', #16968, 1.500000000000001554 ) ;
#12769 = ADVANCED_FACE ( 'NONE', ( #2285 ), #8279, .F. ) ;
#12770 = CIRCLE ( 'NONE', #1296, 1.500000000000000888 ) ;
#12771 = EDGE_CURVE ( 'NONE', #8399, #968, #937, .T. ) ;
#12772 = CARTESIAN_POINT ( 'NONE',  ( 1.360103686702108128, -20.03404830722672259, 8.660254037844412167 ) ) ;
#12773 = ORIENTED_EDGE ( 'NONE', *, *, #1108, .T. ) ;
#12774 = VERTEX_POINT ( 'NONE', #3601 ) ;
#12775 = PRESENTATION_LAYER_ASSIGNMENT (  '', '', ( #13069 ) ) ;
#12776 = DIRECTION ( 'NONE',  ( -0.1566598588826321747, 0.9876526153536343555, 0.000000000000000000 ) ) ;
#12777 = VERTEX_POINT ( 'NONE', #16817 ) ;
#12778 = PLANE ( 'NONE',  #18257 ) ;
#12779 = VECTOR ( 'NONE', #11278, 1000.000000000000000 ) ;
#12780 = DIRECTION ( 'NONE',  ( -0.000000000000000000, -0.000000000000000000, -1.000000000000000000 ) ) ;
#12781 = DIRECTION ( 'NONE',  ( -0.1566598588826321192, 0.9876526153536342445, 7.798540720466730171E-17 ) ) ;
#12782 = DIRECTION ( 'NONE',  ( -0.1615579233078775490, 0.9868632313631133801, 0.000000000000000000 ) ) ;
#12783 = CARTESIAN_POINT ( 'NONE',  ( -35.67686938905902849, -25.90879301532540779, 4.330127018922217630 ) ) ;
#12784 = FACE_OUTER_BOUND ( 'NONE', #6735, .T. ) ;
#12785 = VERTEX_POINT ( 'NONE', #6769 ) ;
#12786 = DIRECTION ( 'NONE',  ( 0.000000000000000000, 0.000000000000000000, 1.000000000000000000 ) ) ;
#12787 = DIRECTION ( 'NONE',  ( -0.1566598588826321192, 0.9876526153536342445, 7.798540720466731404E-17 ) ) ;
#12788 = DIRECTION ( 'NONE',  ( -0.1566598588826321192, 0.9876526153536342445, 7.798540720466730171E-17 ) ) ;
#12789 = CARTESIAN_POINT ( 'NONE',  ( -67.73594437787414790, -88.69941986535906153, 4.330127018922213189 ) ) ;
#12790 = ORIENTED_EDGE ( 'NONE', *, *, #131, .T. ) ;
#12791 = EDGE_CURVE ( 'NONE', #15850, #14394, #12091, .T. ) ;
#12792 = EDGE_LOOP ( 'NONE', ( #4733, #10227 ) ) ;
#12793 = ORIENTED_EDGE ( 'NONE', *, *, #19, .T. ) ;
#12794 = ADVANCED_FACE ( 'NONE', ( #2577 ), #9412, .F. ) ;
#12795 = CARTESIAN_POINT ( 'NONE',  ( -39.09401853261888959, -84.15628395776273862, 1.424741226644455312E-14 ) ) ;
#12796 = AXIS2_PLACEMENT_3D ( 'NONE', #17689, #6293, #696 ) ;
#12797 = ORIENTED_EDGE ( 'NONE', *, *, #17686, .T. ) ;
#12798 = ORIENTED_EDGE ( 'NONE', *, *, #12221, .T. ) ;
#12799 = DIRECTION ( 'NONE',  ( -0.1566598588826321747, 0.9876526153536343555, 0.000000000000000000 ) ) ;
#12800 = ADVANCED_FACE ( 'NONE', ( #2495 ), #6859, .F. ) ;
#12801 = ORIENTED_EDGE ( 'NONE', *, *, #5302, .T. ) ;
#12802 = DIRECTION ( 'NONE',  ( -0.9876526153536336894, -0.1566598588826349503, 0.000000000000000000 ) ) ;
#12803 = CARTESIAN_POINT ( 'NONE',  ( -45.55339554259533230, -27.47539160415171722, -12.99038105676658006 ) ) ;
#12804 = ORIENTED_EDGE ( 'NONE', *, *, #15064, .T. ) ;
#12805 = CIRCLE ( 'NONE', #14325, 1.499999999999999556 ) ;
#12806 = CARTESIAN_POINT ( 'NONE',  ( -63.78533391645962780, -88.07278042982854060, 17.32050807568881368 ) ) ;
#12807 = FACE_BOUND ( 'NONE', #16221, .T. ) ;
#12808 = CARTESIAN_POINT ( 'NONE',  ( -74.19532138785061193, -32.01852751174804013, 17.32050807568881723 ) ) ;
#12809 = CARTESIAN_POINT ( 'NONE',  ( -57.36559191666103175, -87.05449134709142811, 17.32050807568881368 ) ) ;
#12810 = CARTESIAN_POINT ( 'NONE',  ( -57.89905323451571206, -29.43363984018462176, -17.32050807568878170 ) ) ;
#12811 = FACE_OUTER_BOUND ( 'NONE', #17411, .T. ) ;
#12812 = DIRECTION ( 'NONE',  ( -0.9876526153536336894, -0.1566598588826349503, 0.000000000000000000 ) ) ;
#12813 = ORIENTED_EDGE ( 'NONE', *, *, #16350, .F. ) ;
#12814 = ORIENTED_EDGE ( 'NONE', *, *, #13562, .F. ) ;
#12815 = VERTEX_POINT ( 'NONE', #8177 ) ;
#12816 = ORIENTED_EDGE ( 'NONE', *, *, #15768, .F. ) ;
#12817 = CARTESIAN_POINT ( 'NONE',  ( -41.56315007100294423, -84.54793360496933019, 21.65063509461101532 ) ) ;
#12818 = AXIS2_PLACEMENT_3D ( 'NONE', #7567, #1960, #7667 ) ;
#12819 = EDGE_CURVE ( 'NONE', #13293, #7092, #1242, .T. ) ;
#12820 = EDGE_LOOP ( 'NONE', ( #7535, #18568, #5348, #18251 ) ) ;
#12821 = CARTESIAN_POINT ( 'NONE',  ( -62.00000000000000000, 0.000000000000000000, -25.00000000000000000 ) ) ;
#12822 = CARTESIAN_POINT ( 'NONE',  ( -59.79999999999999716, 0.000000000000000000, -20.00000000000000000 ) ) ;
#12823 = EDGE_CURVE ( 'NONE', #11838, #1622, #3613, .T. ) ;
#12824 = DIRECTION ( 'NONE',  ( 0.000000000000000000, 0.000000000000000000, 1.000000000000000000 ) ) ;
#12825 = CYLINDRICAL_SURFACE ( 'NONE', #10274, 2.199999999999993516 ) ;
#12826 = DIRECTION ( 'NONE',  ( 0.000000000000000000, 0.000000000000000000, 1.000000000000000000 ) ) ;
#12827 = CARTESIAN_POINT ( 'NONE',  ( -174.6164565666191777, 55.77096170148206511, 4.052748550462854205 ) ) ;
#12828 = CARTESIAN_POINT ( 'NONE',  ( -306.1404785418517918, -2.850701963179328668, 12.83663829214476237 ) ) ;
#12829 = DIRECTION ( 'NONE',  ( -0.9876526153536341335, -0.1566598588826327021, 0.000000000000000000 ) ) ;
#12830 = CARTESIAN_POINT ( 'NONE',  ( -172.7326993491721225, 43.83249341393818810, 9.951701414186830458E-16 ) ) ;
#12831 = ORIENTED_EDGE ( 'NONE', *, *, #3787, .F. ) ;
#12832 = EDGE_LOOP ( 'NONE', ( #2923, #12019, #12914, #17396 ) ) ;
#12833 = DIRECTION ( 'NONE',  ( -0.1566598588826321192, 0.9876526153536342445, 7.798540720466730171E-17 ) ) ;
#12834 = CARTESIAN_POINT ( 'NONE',  ( -49.01017969633302584, -28.02370111024093191, 4.330127018922217630 ) ) ;
#12835 = DIRECTION ( 'NONE',  ( -0.1566598588826321192, 0.9876526153536342445, 7.798540720466730171E-17 ) ) ;
#12836 = DIRECTION ( 'NONE',  ( 1.000000000000000000, 0.000000000000000000, 0.000000000000000000 ) ) ;
#12837 = ORIENTED_EDGE ( 'NONE', *, *, #8729, .T. ) ;
#12838 = DIRECTION ( 'NONE',  ( -0.1566598588826321192, 0.9876526153536342445, 7.798540720466731404E-17 ) ) ;
#12839 = EDGE_CURVE ( 'NONE', #14985, #6009, #6392, .T. ) ;
#12840 = EDGE_CURVE ( 'NONE', #4741, #10340, #5149, .T. ) ;
#12841 = DIRECTION ( 'NONE',  ( 0.000000000000000000, 0.000000000000000000, 1.000000000000000000 ) ) ;
#12842 = EDGE_CURVE ( 'NONE', #8644, #11461, #12427, .T. ) ;
#12843 = EDGE_LOOP ( 'NONE', ( #305, #8308 ) ) ;
#12844 = FACE_OUTER_BOUND ( 'NONE', #14275, .T. ) ;
#12845 = CIRCLE ( 'NONE', #8914, 1.499999999999999556 ) ;
#12846 = FACE_OUTER_BOUND ( 'NONE', #11542, .T. ) ;
#12847 = ORIENTED_EDGE ( 'NONE', *, *, #8465, .T. ) ;
#12848 = DIRECTION ( 'NONE',  ( -0.9876526153536341335, -0.1566598588826327021, 0.000000000000000000 ) ) ;
#12849 = EDGE_LOOP ( 'NONE', ( #1149, #4590, #16911, #15299 ) ) ;
#12850 = LINE ( 'NONE', #18694, #1424 ) ;
#12851 = DIRECTION ( 'NONE',  ( -0.1566598588826321747, 0.9876526153536343555, 0.000000000000000000 ) ) ;
#12852 = DIRECTION ( 'NONE',  ( -0.9876526153536336894, -0.1566598588826349503, 0.000000000000000000 ) ) ;
#12853 = ORIENTED_EDGE ( 'NONE', *, *, #9124, .F. ) ;
#12854 = DIRECTION ( 'NONE',  ( -0.1566598588826321192, 0.9876526153536342445, 7.798540720466731404E-17 ) ) ;
#12855 = VERTEX_POINT ( 'NONE', #891 ) ;
#12856 = EDGE_CURVE ( 'NONE', #5835, #15309, #16363, .T. ) ;
#12857 = LINE ( 'NONE', #18703, #4531 ) ;
#12858 = VECTOR ( 'NONE', #13682, 1000.000000000000000 ) ;
#12859 = ORIENTED_EDGE ( 'NONE', *, *, #17170, .T. ) ;
#12860 = ADVANCED_FACE ( 'NONE', ( #18360 ), #1179, .F. ) ;
#12861 = EDGE_CURVE ( 'NONE', #794, #7971, #16684, .T. ) ;
#12862 = ORIENTED_EDGE ( 'NONE', *, *, #6874, .T. ) ;
#12863 = DIRECTION ( 'NONE',  ( -0.1566598588826321747, 0.9876526153536343555, 0.000000000000000000 ) ) ;
#12864 = DIRECTION ( 'NONE',  ( -0.2333333333333372228, 0.9723968097209871875, 0.000000000000000000 ) ) ;
#12865 = FACE_OUTER_BOUND ( 'NONE', #18123, .T. ) ;
#12866 = CARTESIAN_POINT ( 'NONE',  ( -61.84966369593023217, -30.06027927571513914, 21.65063509461101887 ) ) ;
#12867 = CARTESIAN_POINT ( 'NONE',  ( -105.9742111339482307, -32.54855632894931716, 2.500000000000000000 ) ) ;
#12868 = CYLINDRICAL_SURFACE ( 'NONE', #6637, 1.500000000000000888 ) ;
#12869 = AXIS2_PLACEMENT_3D ( 'NONE', #10542, #16339, #8181 ) ;
#12870 = CARTESIAN_POINT ( 'NONE',  ( -46.33669483700847280, -22.53712852738359373, 12.99038105676661736 ) ) ;
#12871 = DIRECTION ( 'NONE',  ( 0.9201637183752250371, -0.3915338189555017667, 3.511704013281690619E-17 ) ) ;
#12872 = CARTESIAN_POINT ( 'NONE',  ( -70.20507591625822386, -89.09106951256563889, 1.424741226644455312E-14 ) ) ;
#12873 = ORIENTED_EDGE ( 'NONE', *, *, #17387, .F. ) ;
#12874 = VERTEX_POINT ( 'NONE', #18559 ) ;
#12875 = LINE ( 'NONE', #1262, #12057 ) ;
#12876 = CYLINDRICAL_SURFACE ( 'NONE', #17263, 1.500000000000001554 ) ;
#12877 = ORIENTED_EDGE ( 'NONE', *, *, #13082, .T. ) ;
#12878 = ORIENTED_EDGE ( 'NONE', *, *, #13670, .F. ) ;
#12879 = CARTESIAN_POINT ( 'NONE',  ( -172.0951522251743029, 56.61964399677356141, 2.500000000000000000 ) ) ;
#12880 = VERTEX_POINT ( 'NONE', #1449 ) ;
#12881 = AXIS2_PLACEMENT_3D ( 'NONE', #13236, #5598, #8542 ) ;
#12882 = VERTEX_POINT ( 'NONE', #17299 ) ;
#12883 = CARTESIAN_POINT ( 'NONE',  ( -81.73462711737164454, 33.01666666666666572, -35.00000000000000000 ) ) ;
#12884 = CARTESIAN_POINT ( 'NONE',  ( -21.64537945316773460, -18.62063205531779531, -4.330127018922180326 ) ) ;
#12885 = VERTEX_POINT ( 'NONE', #18651 ) ;
#12886 = EDGE_CURVE ( 'NONE', #13905, #3864, #5621, .T. ) ;
#12887 = EDGE_CURVE ( 'NONE', #13318, #3651, #8790, .T. ) ;
#12888 = AXIS2_PLACEMENT_3D ( 'NONE', #6563, #5414, #3777 ) ;
#12889 = FACE_BOUND ( 'NONE', #12295, .T. ) ;
#12890 = CARTESIAN_POINT ( 'NONE',  ( -41.60278508118079799, -26.84875216862118918, 17.32050807568881723 ) ) ;
#12891 = AXIS2_PLACEMENT_3D ( 'NONE', #5481, #11241, #7190 ) ;
#12892 = DIRECTION ( 'NONE',  ( -0.9876526153536336894, -0.1566598588826349503, 0.000000000000000000 ) ) ;
#12893 = FACE_OUTER_BOUND ( 'NONE', #3443, .T. ) ;
#12894 = ORIENTED_EDGE ( 'NONE', *, *, #12594, .F. ) ;
#12895 = ORIENTED_EDGE ( 'NONE', *, *, #11748, .F. ) ;
#12896 = ORIENTED_EDGE ( 'NONE', *, *, #17096, .T. ) ;
#12897 = VERTEX_POINT ( 'NONE', #12890 ) ;
#12898 = DIRECTION ( 'NONE',  ( 0.000000000000000000, 0.000000000000000000, 1.000000000000000000 ) ) ;
#12899 = VECTOR ( 'NONE', #13076, 1000.000000000000000 ) ;
#12900 = DIRECTION ( 'NONE',  ( -0.1566598588826321192, 0.9876526153536342445, 7.798540720466730171E-17 ) ) ;
#12901 = CARTESIAN_POINT ( 'NONE',  ( 55.85952145814821534, 6.938893903907228378E-15, 30.00000000000000000 ) ) ;
#12902 = AXIS2_PLACEMENT_3D ( 'NONE', #11111, #816, #16541 ) ;
#12903 = VECTOR ( 'NONE', #17452, 1000.000000000000114 ) ;
#12904 = CARTESIAN_POINT ( 'NONE',  ( -19.87442754340095519, -23.40223527320329922, -8.660254037844380193 ) ) ;
#12905 = EDGE_CURVE ( 'NONE', #17960, #584, #4283, .T. ) ;
#12906 = AXIS2_PLACEMENT_3D ( 'NONE', #3452, #7937, #3647 ) ;
#12907 = DIRECTION ( 'NONE',  ( -0.1566598588826321192, 0.9876526153536342445, 7.798540720466730171E-17 ) ) ;
#12908 = APPLICATION_PROTOCOL_DEFINITION ( 'draft international standard', 'automotive_design', 1998, #12682 ) ;
#12909 = AXIS2_PLACEMENT_3D ( 'NONE', #9526, #15298, #8100 ) ;
#12910 = EDGE_CURVE ( 'NONE', #10192, #17580, #14337, .T. ) ;
#12911 = CARTESIAN_POINT ( 'NONE',  ( -173.4308285199811905, 56.32218110407216471, 2.822349119005441054 ) ) ;
#12912 = CARTESIAN_POINT ( 'NONE',  ( -43.86756329862440396, -22.14547888017701283, 8.660254037844417496 ) ) ;
#12913 = FACE_BOUND ( 'NONE', #9274, .T. ) ;
#12914 = ORIENTED_EDGE ( 'NONE', *, *, #8979, .T. ) ;
#12915 = ORIENTED_EDGE ( 'NONE', *, *, #13738, .T. ) ;
#12916 = FACE_BOUND ( 'NONE', #16156, .T. ) ;
#12917 = CARTESIAN_POINT ( 'NONE',  ( -37.61253960958842413, -83.92129416943879505, 8.660254037844412167 ) ) ;
#12918 = AXIS2_PLACEMENT_3D ( 'NONE', #11585, #17406, #18759 ) ;
#12919 = ADVANCED_FACE ( 'NONE', ( #7414 ), #18735, .F. ) ;
#12920 = FACE_OUTER_BOUND ( 'NONE', #11649, .T. ) ;
#12921 = VERTEX_POINT ( 'NONE', #17197 ) ;
#12922 = ORIENTED_EDGE ( 'NONE', *, *, #14304, .F. ) ;
#12923 = DIRECTION ( 'NONE',  ( 0.000000000000000000, 0.000000000000000000, 1.000000000000000000 ) ) ;
#12924 = VECTOR ( 'NONE', #15604, 1000.000000000000000 ) ;
#12925 = CARTESIAN_POINT ( 'NONE',  ( -28.26947477390680774, -24.73384407370567217, -17.32050807568878170 ) ) ;
#12926 = CARTESIAN_POINT ( 'NONE',  ( -75.96627329761737712, -27.23692429386253266, -12.99038105676658006 ) ) ;
#12927 = CARTESIAN_POINT ( 'NONE',  ( 2.058283315319403783, -14.86079544213463066, 1.406148482768655632E-14 ) ) ;
#12928 = FACE_OUTER_BOUND ( 'NONE', #6158, .T. ) ;
#12929 = DIRECTION ( 'NONE',  ( -0.9876526153536341335, -0.1566598588826327021, 0.000000000000000000 ) ) ;
#12930 =( NAMED_UNIT ( * ) PLANE_ANGLE_UNIT ( ) SI_UNIT ( $, .RADIAN. ) );
#12931 = CIRCLE ( 'NONE', #15966, 1.500000000000001332 ) ;
#12932 = ADVANCED_FACE ( 'NONE', ( #15643 ), #1636, .F. ) ;
#12933 = CARTESIAN_POINT ( 'NONE',  ( -44.03228160938704860, -84.93958325217589334, -17.32050807568878525 ) ) ;
#12934 = LINE ( 'NONE', #14382, #16882 ) ;
#12935 = CARTESIAN_POINT ( 'NONE',  ( -44.03228160938704860, -84.93958325217589334, -8.660254037844385522 ) ) ;
#12936 = DIRECTION ( 'NONE',  ( -0.1566598588826321192, 0.9876526153536342445, 7.798540720466730171E-17 ) ) ;
#12937 = EDGE_LOOP ( 'NONE', ( #10624, #4954, #2212, #16761, #16942, #9012 ) ) ;
#12938 = DIRECTION ( 'NONE',  ( -0.1566598588826321192, 0.9876526153536342445, 7.798540720466730171E-17 ) ) ;
#12939 = AXIS2_PLACEMENT_3D ( 'NONE', #12582, #5694, #18442 ) ;
#12940 = ORIENTED_EDGE ( 'NONE', *, *, #3450, .F. ) ;
#12942 = ORIENTED_EDGE ( 'NONE', *, *, #14636, .T. ) ;
#12941 = FACE_OUTER_BOUND ( 'NONE', #7321, .T. ) ;
#12943 = EDGE_CURVE ( 'NONE', #13071, #5613, #633, .T. ) ;
#12944 = AXIS2_PLACEMENT_3D ( 'NONE', #14289, #8604, #5767 ) ;
#12945 = CARTESIAN_POINT ( 'NONE',  ( 3.133606229046292935, -19.12225244224100962, 24.99999999999998934 ) ) ;
#12946 = ADVANCED_FACE ( 'NONE', ( #12987 ), #8734, .F. ) ;
#12947 = EDGE_LOOP ( 'NONE', ( #13302, #397 ) ) ;
#12948 = AXIS2_PLACEMENT_3D ( 'NONE', #12867, #17443, #8624 ) ;
#12949 = CARTESIAN_POINT ( 'NONE',  ( -170.4124675745486570, 31.54971992778987655, 2.500000000000000000 ) ) ;
#12950 = DIRECTION ( 'NONE',  ( -0.000000000000000000, -0.000000000000000000, -1.000000000000000000 ) ) ;
#12951 = CARTESIAN_POINT ( 'NONE',  ( -20.16390053013728334, -18.38564226699385529, 21.65063509461101177 ) ) ;
#12952 = EDGE_CURVE ( 'NONE', #626, #18004, #4458, .T. ) ;
#12953 = CIRCLE ( 'NONE', #4180, 1.500000000000000888 ) ;
#12954 = VERTEX_POINT ( 'NONE', #2670 ) ;
#12955 = CARTESIAN_POINT ( 'NONE',  ( -65.23030399291525327, 43.49999999999997868, 110.7545852194966045 ) ) ;
#12956 = CARTESIAN_POINT ( 'NONE',  ( -7.034943543803747090, -21.36565710772908488, -8.660254037844380193 ) ) ;
#12957 = VECTOR ( 'NONE', #4002, 1000.000000000000000 ) ;
#12958 = LINE ( 'NONE', #7393, #6333 ) ;
#12959 = AXIS2_PLACEMENT_3D ( 'NONE', #4099, #7084, #18294 ) ;
#12960 = DIRECTION ( 'NONE',  ( -0.9876526153536341335, -0.1566598588826327021, 0.000000000000000000 ) ) ;
#12961 = EDGE_CURVE ( 'NONE', #9249, #3229, #15149, .T. ) ;
#12962 = DIRECTION ( 'NONE',  ( -0.9876526153536344665, -0.1566598588826304539, 0.000000000000000000 ) ) ;
#12963 = EDGE_CURVE ( 'NONE', #15692, #4549, #17601, .T. ) ;
#12964 = CARTESIAN_POINT ( 'NONE',  ( -48.80582637539256297, -22.92877817459016754, 1.908195823574487804E-14 ) ) ;
#12965 = DIRECTION ( 'NONE',  ( -0.1566598588826321192, 0.9876526153536342445, 7.798540720466730171E-17 ) ) ;
#12967 = ORIENTED_EDGE ( 'NONE', *, *, #2271, .F. ) ;
#12966 = DIRECTION ( 'NONE',  ( -0.1566598588826321192, 0.9876526153536342445, 7.798540720466731404E-17 ) ) ;
#12968 = EDGE_CURVE ( 'NONE', #14954, #2218, #5473, .T. ) ;
#12969 = VECTOR ( 'NONE', #5978, 1000.000000000000000 ) ;
#12970 = ORIENTED_EDGE ( 'NONE', *, *, #81, .T. ) ;
#12971 = CARTESIAN_POINT ( 'NONE',  ( -79.24244631363546887, 32.81909429640987952, 35.00000000000000000 ) ) ;
#12972 = EDGE_LOOP ( 'NONE', ( #17165, #2029, #7733, #11254 ) ) ;
#12973 = VERTEX_POINT ( 'NONE', #1548 ) ;
#12974 = ORIENTED_EDGE ( 'NONE', *, *, #7447, .T. ) ;
#12975 = CARTESIAN_POINT ( 'NONE',  ( -23.33121169713865584, -23.95054477929251036, -17.32050807568878170 ) ) ;
#12976 = AXIS2_PLACEMENT_3D ( 'NONE', #10851, #7848, #12373 ) ;
#12977 = FACE_BOUND ( 'NONE', #3742, .T. ) ;
#12978 = CARTESIAN_POINT ( 'NONE',  ( -24.11451099155181055, -19.01228170252437977, 8.660254037844417496 ) ) ;
#12979 = AXIS2_PLACEMENT_3D ( 'NONE', #16144, #3057, #3137 ) ;
#12980 = DIRECTION ( 'NONE',  ( -2.671473304378624222E-16, -0.000000000000000000, -1.000000000000000000 ) ) ;
#12981 = AXIS2_PLACEMENT_3D ( 'NONE', #11445, #8634, #2841 ) ;
#12982 = DIRECTION ( 'NONE',  ( 0.000000000000000000, 0.000000000000000000, 1.000000000000000000 ) ) ;
#12983 = EDGE_LOOP ( 'NONE', ( #16768, #8182 ) ) ;
#12984 = AXIS2_PLACEMENT_3D ( 'NONE', #15518, #16967, #1228 ) ;
#12985 = EDGE_CURVE ( 'NONE', #18075, #6856, #14252, .T. ) ;
#12986 = VERTEX_POINT ( 'NONE', #10239 ) ;
#12987 = FACE_OUTER_BOUND ( 'NONE', #17059, .T. ) ;
#12988 = CIRCLE ( 'NONE', #10808, 1.500000000000000888 ) ;
#12989 = VECTOR ( 'NONE', #1109, 1000.000000000000000 ) ;
#12990 = AXIS2_PLACEMENT_3D ( 'NONE', #7279, #4500, #13210 ) ;
#12991 = DIRECTION ( 'NONE',  ( -0.1566598588826321192, 0.9876526153536342445, 7.798540720466730171E-17 ) ) ;
#12992 = CARTESIAN_POINT ( 'NONE',  ( -169.7848337124965212, 44.38934903984782210, -5.500000000000000000 ) ) ;
#12993 = CARTESIAN_POINT ( 'NONE',  ( -64.31879523431432233, -30.45192892292171294, 8.660254037844417496 ) ) ;
#12994 = ORIENTED_EDGE ( 'NONE', *, *, #6488, .F. ) ;
#12995 = ADVANCED_FACE ( 'NONE', ( #8833 ), #9869, .F. ) ;
#12996 = ADVANCED_FACE ( 'NONE', ( #8563 ), #1908, .F. ) ;
#12997 = EDGE_LOOP ( 'NONE', ( #7366, #13299, #11194, #1022 ) ) ;
#12998 = VECTOR ( 'NONE', #7163, 1000.000000000000000 ) ;
#12999 = ORIENTED_EDGE ( 'NONE', *, *, #13245, .T. ) ;
#13000 = DIRECTION ( 'NONE',  ( 0.000000000000000000, 0.000000000000000000, 1.000000000000000000 ) ) ;
#13001 = ORIENTED_EDGE ( 'NONE', *, *, #7255, .F. ) ;
#13002 = AXIS2_PLACEMENT_3D ( 'NONE', #4580, #2015, #7434 ) ;
#13003 = LINE ( 'NONE', #5992, #13661 ) ;
#13004 = CARTESIAN_POINT ( 'NONE',  ( -68.76323200340563346, -31.15689828789355786, 4.330127018922217630 ) ) ;
#13005 = AXIS2_PLACEMENT_3D ( 'NONE', #3256, #9159, #6421 ) ;
#13006 = ORIENTED_EDGE ( 'NONE', *, *, #4968, .F. ) ;
#13007 = AXIS2_PLACEMENT_3D ( 'NONE', #5071, #3547, #12367 ) ;
#13008 = LINE ( 'NONE', #10074, #17235 ) ;
#13009 = DIRECTION ( 'NONE',  ( -0.1566598588826321747, 0.9876526153536343555, 0.000000000000000000 ) ) ;
#13010 = APPLICATION_PROTOCOL_DEFINITION ( 'draft international standard', 'automotive_design', 1998, #10387 ) ;
#13011 = DIRECTION ( 'NONE',  ( -0.9876526153536336894, -0.1566598588826350336, 0.000000000000000000 ) ) ;
#13012 = CIRCLE ( 'NONE', #5780, 1.500000000000000000 ) ;
#13013 = DIRECTION ( 'NONE',  ( -0.1566598588826321747, 0.9876526153536343555, 0.000000000000000000 ) ) ;
#13014 = AXIS2_PLACEMENT_3D ( 'NONE', #3505, #7897, #10641 ) ;
#13015 = ORIENTED_EDGE ( 'NONE', *, *, #4340, .F. ) ;
#13016 = ORIENTED_EDGE ( 'NONE', *, *, #10173, .T. ) ;
#13017 = FACE_BOUND ( 'NONE', #4939, .T. ) ;
#13018 = CYLINDRICAL_SURFACE ( 'NONE', #14173, 1.500000000000001554 ) ;
#13019 = ORIENTED_EDGE ( 'NONE', *, *, #13395, .F. ) ;
#13020 = AXIS2_PLACEMENT_3D ( 'NONE', #7091, #1484, #13024 ) ;
#13021 = ADVANCED_FACE ( 'NONE', ( #9206 ), #15068, .F. ) ;
#13022 = CARTESIAN_POINT ( 'NONE',  ( -36.46016868347218320, -20.97052993855728076, 21.65063509461102242 ) ) ;
#13023 = EDGE_CURVE ( 'NONE', #3313, #10907, #18356, .T. ) ;
#13024 = DIRECTION ( 'NONE',  ( -0.9876526153536336894, -0.1566598588826349503, 0.000000000000000000 ) ) ;
#13025 = EDGE_LOOP ( 'NONE', ( #510, #7558, #13825, #5782 ) ) ;
#13026 = LINE ( 'NONE', #10276, #3056 ) ;
#13027 = AXIS2_PLACEMENT_3D ( 'NONE', #15288, #7915, #4949 ) ;
#13028 = EDGE_CURVE ( 'NONE', #4155, #14517, #446, .T. ) ;
#13029 = AXIS2_PLACEMENT_3D ( 'NONE', #4785, #9059, #15021 ) ;
#13030 = DIRECTION ( 'NONE',  ( -0.1566598588826321192, 0.9876526153536342445, 7.798540720466731404E-17 ) ) ;
#13031 = FACE_OUTER_BOUND ( 'NONE', #11718, .T. ) ;
#13032 = DIRECTION ( 'NONE',  ( 0.000000000000000000, 0.000000000000000000, 1.000000000000000000 ) ) ;
#13033 = VECTOR ( 'NONE', #10366, 1000.000000000000000 ) ;
#13034 = ORIENTED_EDGE ( 'NONE', *, *, #3694, .F. ) ;
#13035 = CYLINDRICAL_SURFACE ( 'NONE', #14203, 1.500000000000001554 ) ;
#13036 = CARTESIAN_POINT ( 'NONE',  ( -90.00000000000001421, 34.99999999999999289, 30.00000000000002842 ) ) ;
#13037 = VECTOR ( 'NONE', #14352, 1000.000000000000000 ) ;
#13038 = CARTESIAN_POINT ( 'NONE',  ( -40.57549745564935506, -84.39127374608668219, -17.32050807568878525 ) ) ;
#13039 = EDGE_LOOP ( 'NONE', ( #10625, #18661, #3643, #13831 ) ) ;
#13040 = DIRECTION ( 'NONE',  ( 0.000000000000000000, 0.000000000000000000, 1.000000000000000000 ) ) ;
#13042 = VERTEX_POINT ( 'NONE', #6091 ) ;
#13041 = FACE_OUTER_BOUND ( 'NONE', #2345, .T. ) ;
#13043 = AXIS2_PLACEMENT_3D ( 'NONE', #7994, #18370, #801 ) ;
#13044 = CARTESIAN_POINT ( 'NONE',  ( 2.000000000000000000, 2.449293598294706414E-16, -30.00000000000000000 ) ) ;
#13045 = DIRECTION ( 'NONE',  ( -0.1566598588826321470, 0.9876526153536342445, 4.523475108491707377E-17 ) ) ;
#13046 = EDGE_LOOP ( 'NONE', ( #11737, #140, #461, #18350 ) ) ;
#13047 = VERTEX_POINT ( 'NONE', #11836 ) ;
#13048 = AXIS2_PLACEMENT_3D ( 'NONE', #10814, #3246, #16357 ) ;
#13049 = EDGE_LOOP ( 'NONE', ( #5696, #18328 ) ) ;
#13050 = EDGE_CURVE ( 'NONE', #17941, #4280, #1814, .T. ) ;
#13051 = CARTESIAN_POINT ( 'NONE',  ( -349.5448134615015761, 26.54870825572371018, 2.934543024899866731E-15 ) ) ;
#13052 = CIRCLE ( 'NONE', #15487, 1.499999999999999556 ) ;
#13053 = AXIS2_PLACEMENT_3D ( 'NONE', #3326, #9130, #1923 ) ;
#13054 = CYLINDRICAL_SURFACE ( 'NONE', #18635, 150.0000000000000284 ) ;
#13055 = CARTESIAN_POINT ( 'NONE',  ( -26.74836084069850983, -82.19803572172985184, 4.330127018922213189 ) ) ;
#13056 = FACE_BOUND ( 'NONE', #12843, .T. ) ;
#13057 = ADVANCED_FACE ( 'NONE', ( #587 ), #10619, .F. ) ;
#13058 = CARTESIAN_POINT ( 'NONE',  ( -17.40529600501687923, -23.01058562599671831, -12.99038105676658006 ) ) ;
#13059 = AXIS2_PLACEMENT_3D ( 'NONE', #676, #17947, #10696 ) ;
#13060 = CARTESIAN_POINT ( 'NONE',  ( -68.76323200340563346, -31.15689828789355786, -12.99038105676658006 ) ) ;
#13061 = ORIENTED_EDGE ( 'NONE', *, *, #4294, .F. ) ;
#13062 = DIRECTION ( 'NONE',  ( -0.9792327305835186735, -0.2027393877714586679, 0.000000000000000000 ) ) ;
#13063 = AXIS2_PLACEMENT_3D ( 'NONE', #8479, #1460, #8745 ) ;
#13064 = CARTESIAN_POINT ( 'NONE',  ( -1.109027851681973598, -20.42569795443330349, -21.65063509461098334 ) ) ;
#13065 = PLANE ( 'NONE',  #11169 ) ;
#13066 = CARTESIAN_POINT ( 'NONE',  ( -137.7298645655810390, -88.63485219053825404, 2.500000000000000000 ) ) ;
#13068 = EDGE_LOOP ( 'NONE', ( #16658, #17769 ) ) ;
#13067 = DIRECTION ( 'NONE',  ( -0.9876526153536341335, -0.1566598588826327021, 0.000000000000000000 ) ) ;
#13069 = STYLED_ITEM ( 'NONE', ( #9285 ), #2591 ) ;
#13070 = VERTEX_POINT ( 'NONE', #7502 ) ;
#13071 = VERTEX_POINT ( 'NONE', #16135 ) ;
#13072 = DIRECTION ( 'NONE',  ( -0.1566598588826321192, 0.9876526153536342445, 7.798540720466730171E-17 ) ) ;
#13073 = ORIENTED_EDGE ( 'NONE', *, *, #957, .T. ) ;
#13074 = ORIENTED_EDGE ( 'NONE', *, *, #11854, .F. ) ;
#13075 = VERTEX_POINT ( 'NONE', #16313 ) ;
#13076 = DIRECTION ( 'NONE',  ( -0.1566598588826321192, 0.9876526153536342445, 7.798540720466730171E-17 ) ) ;
#13077 = AXIS2_PLACEMENT_3D ( 'NONE', #2834, #7390, #1425 ) ;
#13078 = ORIENTED_EDGE ( 'NONE', *, *, #11613, .F. ) ;
#13079 = ORIENTED_EDGE ( 'NONE', *, *, #1759, .T. ) ;
#13080 = CARTESIAN_POINT ( 'NONE',  ( -21.64537945316773460, -18.62063205531779886, 12.99038105676661736 ) ) ;
#13081 = ORIENTED_EDGE ( 'NONE', *, *, #704, .F. ) ;
#13082 = EDGE_CURVE ( 'NONE', #4539, #15554, #16500, .T. ) ;
#13083 = EDGE_CURVE ( 'NONE', #13047, #7914, #17574, .T. ) ;
#13084 = CARTESIAN_POINT ( 'NONE',  ( -76.91617387511415416, -2.073484822433842911, -7.028799330061641371 ) ) ;
#13085 = EDGE_CURVE ( 'NONE', #13701, #3470, #7127, .T. ) ;
#13086 = CYLINDRICAL_SURFACE ( 'NONE', #9041, 1.500000000000001554 ) ;
#13087 = EDGE_LOOP ( 'NONE', ( #929, #6454, #16733, #17718 ) ) ;
#13088 = VERTEX_POINT ( 'NONE', #17852 ) ;
#13089 = COLOUR_RGB ( '', 0.40784314, 0.44705882, 0.49803922) ;
#13090 = DIRECTION ( 'NONE',  ( 0.000000000000000000, 0.000000000000000000, 1.000000000000000000 ) ) ;
#13091 = CARTESIAN_POINT ( 'NONE',  ( -65.10209452872746283, -25.51366584615359301, 8.660254037844417496 ) ) ;
#13092 = DIRECTION ( 'NONE',  ( -1.000000000000000000, 0.000000000000000000, 0.000000000000000000 ) ) ;
#13093 = CARTESIAN_POINT ( 'NONE',  ( -2.000000000000000000, 2.449293598294706414E-16, -25.65685424949237614 ) ) ;
#13094 = ORIENTED_EDGE ( 'NONE', *, *, #12195, .F. ) ;
#13095 = EDGE_LOOP ( 'NONE', ( #17045, #7116 ) ) ;
#13096 = EDGE_LOOP ( 'NONE', ( #1057, #448 ) ) ;
#13097 = DIRECTION ( 'NONE',  ( -0.1566598588826321747, 0.9876526153536343555, 0.000000000000000000 ) ) ;
#13098 = EDGE_LOOP ( 'NONE', ( #5745, #16174 ) ) ;
#13099 = CARTESIAN_POINT ( 'NONE',  ( -70.00000000000000000, 44.99999999999999289, 110.7545852194966045 ) ) ;
#13100 = DIRECTION ( 'NONE',  ( 1.000000000000000000, 0.000000000000000000, -2.995206001686573514E-16 ) ) ;
#13101 = EDGE_CURVE ( 'NONE', #8447, #403, #13540, .T. ) ;
#13102 = VERTEX_POINT ( 'NONE', #16422 ) ;
#13103 = CIRCLE ( 'NONE', #14630, 1.500000000000000888 ) ;
#13104 = DIRECTION ( 'NONE',  ( -0.1566598588826321747, 0.9876526153536343555, 0.000000000000000000 ) ) ;
#13105 = EDGE_LOOP ( 'NONE', ( #10076, #1275 ) ) ;
#13106 = CARTESIAN_POINT ( 'NONE',  ( 2.881217619910392269, -77.49823995525089515, -21.65063509461098690 ) ) ;
#13107 = LINE ( 'NONE', #1656, #8351 ) ;
#13108 = ORIENTED_EDGE ( 'NONE', *, *, #16861, .T. ) ;
#13109 = EDGE_LOOP ( 'NONE', ( #8519, #7560 ) ) ;
#13110 = AXIS2_PLACEMENT_3D ( 'NONE', #9174, #365, #6052 ) ;
#13111 = CARTESIAN_POINT ( 'NONE',  ( -137.7298645655810390, -88.63485219053825404, 2.500000000000000000 ) ) ;
#13112 = ORIENTED_EDGE ( 'NONE', *, *, #18780, .T. ) ;
#13113 = ORIENTED_EDGE ( 'NONE', *, *, #1759, .F. ) ;
#13114 = CYLINDRICAL_SURFACE ( 'NONE', #13230, 1.500000000000001554 ) ;
#13115 = EDGE_LOOP ( 'NONE', ( #14930, #5153, #2974, #16124 ) ) ;
#13116 = ORIENTED_EDGE ( 'NONE', *, *, #9023, .F. ) ;
#13117 = CARTESIAN_POINT ( 'NONE',  ( -21.64537945316773460, -18.62063205531779886, 4.330127018922218518 ) ) ;
#13118 = ORIENTED_EDGE ( 'NONE', *, *, #4367, .T. ) ;
#13119 = DIRECTION ( 'NONE',  ( -0.000000000000000000, -0.000000000000000000, -1.000000000000000000 ) ) ;
#13120 = CARTESIAN_POINT ( 'NONE',  ( -6.830590222863280658, -16.27073417207831696, -4.330127018922183879 ) ) ;
#13121 = CARTESIAN_POINT ( 'NONE',  ( -39.13365354279673625, -26.45710252141460828, -12.99038105676658006 ) ) ;
#13122 =( LENGTH_UNIT ( ) NAMED_UNIT ( * ) SI_UNIT ( .MILLI., .METRE. ) );
#13123 = EDGE_CURVE ( 'NONE', #12715, #7418, #17722, .T. ) ;
#13124 = EDGE_CURVE ( 'NONE', #13600, #14719, #4922, .T. ) ;
#13125 = CARTESIAN_POINT ( 'NONE',  ( -20.65772683781411345, -18.46397219643516507, 8.660254037844417496 ) ) ;
#13126 = DIRECTION ( 'NONE',  ( 0.000000000000000000, 0.000000000000000000, 1.000000000000000000 ) ) ;
#13127 = SHAPE_REPRESENTATION ( 'Central Hinge Pivot Pin', ( #18772 ), #4452 ) ;
#13128 = CARTESIAN_POINT ( 'NONE',  ( -58.84707083969148300, -87.28948113541535747, -17.32050807568878525 ) ) ;
#13129 = DIRECTION ( 'NONE',  ( -0.9876526153536336894, -0.1566598588826350336, 0.000000000000000000 ) ) ;
#13130 = ORIENTED_EDGE ( 'NONE', *, *, #8322, .T. ) ;
#13131 = DIRECTION ( 'NONE',  ( 0.000000000000000000, 0.000000000000000000, 1.000000000000000000 ) ) ;
#13132 = EDGE_CURVE ( 'NONE', #10635, #4836, #15575, .T. ) ;
#13133 = ORIENTED_EDGE ( 'NONE', *, *, #17118, .T. ) ;
#13134 = VERTEX_POINT ( 'NONE', #3490 ) ;
#13135 = DIRECTION ( 'NONE',  ( -0.9876526153536336894, -0.1566598588826349503, 0.000000000000000000 ) ) ;
#13136 = ORIENTED_EDGE ( 'NONE', *, *, #5236, .F. ) ;
#13137 = ORIENTED_EDGE ( 'NONE', *, *, #12447, .F. ) ;
#13138 = CARTESIAN_POINT ( 'NONE',  ( -13.25033222266188915, -17.28902325481542235, -4.330127018922180326 ) ) ;
#13139 = CARTESIAN_POINT ( 'NONE',  ( -45.55339554259534651, -27.47539160415172432, -21.65063509461098334 ) ) ;
#13140 = DIRECTION ( 'NONE',  ( -0.9876526153536341335, -0.1566598588826327021, 0.000000000000000000 ) ) ;
#13141 = DIRECTION ( 'NONE',  ( -0.9876526153536336894, -0.1566598588826350336, 0.000000000000000000 ) ) ;
#13142 = DIRECTION ( 'NONE',  ( -1.000000000000000000, 0.000000000000000000, 0.000000000000000000 ) ) ;
#13143 = DIRECTION ( 'NONE',  ( -0.1566598588826321192, 0.9876526153536342445, 7.798540720466730171E-17 ) ) ;
#13144 = ORIENTED_EDGE ( 'NONE', *, *, #4744, .F. ) ;
#13145 = LINE ( 'NONE', #178, #11362 ) ;
#13146 = FACE_BOUND ( 'NONE', #4559, .T. ) ;
#13147 = CARTESIAN_POINT ( 'NONE',  ( 3.231158466157551423, 19.73726462726227737, 30.00000000000000000 ) ) ;
#13148 = CARTESIAN_POINT ( 'NONE',  ( 11.59211860341529565, 6.314490184041233967, 20.00000000000000000 ) ) ;
#13149 = EDGE_CURVE ( 'NONE', #10517, #5280, #15880, .T. ) ;
#13150 = AXIS2_PLACEMENT_3D ( 'NONE', #8053, #12760, #18142 ) ;
#13151 = VERTEX_POINT ( 'NONE', #4560 ) ;
#13152 = EDGE_LOOP ( 'NONE', ( #18788, #10787, #4919, #12006 ) ) ;
#13153 = EDGE_LOOP ( 'NONE', ( #14302, #10980, #14648, #17100 ) ) ;
#13154 = CARTESIAN_POINT ( 'NONE',  ( -25.80034323552273179, -24.34219442649909126, -4.330127018922181215 ) ) ;
#13155 = VERTEX_POINT ( 'NONE', #13261 ) ;
#13156 = EDGE_CURVE ( 'NONE', #15511, #11621, #8003, .T. ) ;
#13157 = ORIENTED_EDGE ( 'NONE', *, *, #11679, .T. ) ;
#13158 = ORIENTED_EDGE ( 'NONE', *, *, #17291, .T. ) ;
#13159 = DIRECTION ( 'NONE',  ( -0.9868632313631133801, -0.1615579233078775490, -2.999697980758351518E-17 ) ) ;
#13160 = EDGE_CURVE ( 'NONE', #10405, #6575, #11016, .T. ) ;
#13161 = CYLINDRICAL_SURFACE ( 'NONE', #6128, 1.500000000000001554 ) ;
#13162 = ORIENTED_EDGE ( 'NONE', *, *, #17168, .F. ) ;
#13163 = DIRECTION ( 'NONE',  ( 0.000000000000000000, 0.000000000000000000, 1.000000000000000000 ) ) ;
#13164 = CIRCLE ( 'NONE', #4980, 3.000000000000000888 ) ;
#13165 = DIRECTION ( 'NONE',  ( -0.1566598588826321747, 0.9876526153536343555, 0.000000000000000000 ) ) ;
#13166 = ORIENTED_EDGE ( 'NONE', *, *, #8662, .T. ) ;
#13167 = ORIENTED_EDGE ( 'NONE', *, *, #11115, .T. ) ;
#13168 = EDGE_CURVE ( 'NONE', #13430, #5005, #4966, .T. ) ;
#13169 = CARTESIAN_POINT ( 'NONE',  ( -65.30644784966793281, -30.60858878180435738, 12.99038105676661736 ) ) ;
#13170 = PLANE ( 'NONE',  #16317 ) ;
#13171 = FACE_BOUND ( 'NONE', #5516, .T. ) ;
#13172 = DIRECTION ( 'NONE',  ( -0.9876526153536341335, -0.1566598588826327021, 0.000000000000000000 ) ) ;
#13173 = CIRCLE ( 'NONE', #4990, 1.499999999999999556 ) ;
#13174 = VERTEX_POINT ( 'NONE', #3684 ) ;
#13175 = EDGE_CURVE ( 'NONE', #13731, #5249, #14664, .T. ) ;
#13176 = ORIENTED_EDGE ( 'NONE', *, *, #5661, .F. ) ;
#13177 = ORIENTED_EDGE ( 'NONE', *, *, #16228, .F. ) ;
#13178 = FACE_OUTER_BOUND ( 'NONE', #16375, .T. ) ;
#13179 = B_SPLINE_CURVE_WITH_KNOTS ( 'NONE', 3,
 ( #1299, #11484, #10162, #11584, #4390, #4482, #12827, #6003, #10262, #14544, #7165, #13188, #12911, #2868, #5739, #8667 ),
 .UNSPECIFIED., .F., .F.,
 ( 4, 2, 2, 2, 2, 2, 2, 4 ),
 ( 1.734723475976807094E-18, 0.0006035471611761495346, 0.001207094322352297334, 0.001810641483528445134, 0.002414188644704592934, 0.003017735805880740734, 0.003621282967056888534, 0.004828377289409252655 ),
 .UNSPECIFIED. ) ;
#13180 = VERTEX_POINT ( 'NONE', #6470 ) ;
#13181 = FACE_BOUND ( 'NONE', #6200, .T. ) ;
#13182 = DIRECTION ( 'NONE',  ( 1.000000000000000000, 1.387778780781444492E-15, 0.000000000000000000 ) ) ;
#13183 = EDGE_LOOP ( 'NONE', ( #8058, #5391, #12197, #16179 ) ) ;
#13184 = DIRECTION ( 'NONE',  ( -0.1566598588826321747, 0.9876526153536343555, 0.000000000000000000 ) ) ;
#13185 = CIRCLE ( 'NONE', #15008, 150.0000000000000284 ) ;
#13186 = CIRCLE ( 'NONE', #5008, 2.200000000000000178 ) ;
#13187 = ORIENTED_EDGE ( 'NONE', *, *, #10826, .T. ) ;
#13188 = CARTESIAN_POINT ( 'NONE',  ( -173.6030297042496500, 56.26981074892695034, 2.921574671186270677 ) ) ;
#13189 = CARTESIAN_POINT ( 'NONE',  ( -2.200000000000000178, 0.000000000000000000, 20.00000000000000000 ) ) ;
#13190 = ADVANCED_FACE ( 'NONE', ( #15810 ), #152, .T. ) ;
#13191 = CARTESIAN_POINT ( 'NONE',  ( -174.8673125818257006, 55.13264502119463373, -5.500000000000001776 ) ) ;
#13192 = LINE ( 'NONE', #5917, #13465 ) ;
#13193 = EDGE_CURVE ( 'NONE', #18229, #14892, #18029, .T. ) ;
#13194 = EDGE_LOOP ( 'NONE', ( #2520, #5320 ) ) ;
#13195 = ORIENTED_EDGE ( 'NONE', *, *, #13835, .F. ) ;
#13196 = FACE_BOUND ( 'NONE', #9116, .T. ) ;
#13197 = CYLINDRICAL_SURFACE ( 'NONE', #4477, 1.500000000000001554 ) ;
#13198 = EDGE_CURVE ( 'NONE', #11470, #15920, #1231, .T. ) ;
#13199 = CIRCLE ( 'NONE', #13781, 2.000000000000000000 ) ;
#13200 = CARTESIAN_POINT ( 'NONE',  ( -57.20087360589840131, -24.26038697509254760, 17.32050807568881723 ) ) ;
#13201 = DIRECTION ( 'NONE',  ( -0.9876526153536341335, -0.1566598588826327021, 0.000000000000000000 ) ) ;
#13202 = ORIENTED_EDGE ( 'NONE', *, *, #3770, .T. ) ;
#13203 = CIRCLE ( 'NONE', #2620, 1.500000000000000000 ) ;
#13204 = ORIENTED_EDGE ( 'NONE', *, *, #463, .F. ) ;
#13205 = VERTEX_POINT ( 'NONE', #11242 ) ;
#13206 = DIRECTION ( 'NONE',  ( 0.000000000000000000, 0.000000000000000000, 1.000000000000000000 ) ) ;
#13207 = AXIS2_PLACEMENT_3D ( 'NONE', #6817, #17147, #8410 ) ;
#13208 = CARTESIAN_POINT ( 'NONE',  ( -26.58364252993588650, -19.40393134973096068, 21.65063509461102242 ) ) ;
#13209 = CIRCLE ( 'NONE', #15635, 2.000000000000000000 ) ;
#13210 = DIRECTION ( 'NONE',  ( 1.000000000000000000, 0.000000000000000000, 0.000000000000000000 ) ) ;
#13211 = DIRECTION ( 'NONE',  ( -0.1566598588826321192, 0.9876526153536342445, 7.798540720466730171E-17 ) ) ;
#13212 = DIRECTION ( 'NONE',  ( -0.1566598588826321747, 0.9876526153536343555, 0.000000000000000000 ) ) ;
#13213 = STYLED_ITEM ( 'NONE', ( #12343 ), #15126 ) ;
#13214 = DIRECTION ( 'NONE',  ( -0.1566598588826321192, 0.9876526153536342445, 7.798540720466730171E-17 ) ) ;
#13215 = VECTOR ( 'NONE', #13797, 1000.000000000000000 ) ;
#13216 = DIRECTION ( 'NONE',  ( 0.1856185419698762329, -0.9826218788918640312, 0.000000000000000000 ) ) ;
#13217 = FACE_OUTER_BOUND ( 'NONE', #9310, .T. ) ;
#13218 = ORIENTED_EDGE ( 'NONE', *, *, #15365, .T. ) ;
#13219 = ORIENTED_EDGE ( 'NONE', *, *, #4173, .T. ) ;
#13220 = DIRECTION ( 'NONE',  ( -1.000000000000000000, 0.000000000000000000, 0.000000000000000000 ) ) ;
#13221 = ORIENTED_EDGE ( 'NONE', *, *, #13050, .F. ) ;
#13222 = ORIENTED_EDGE ( 'NONE', *, *, #15913, .F. ) ;
#13223 = VECTOR ( 'NONE', #11591, 1000.000000000000000 ) ;
#13224 = VERTEX_POINT ( 'NONE', #12205 ) ;
#13225 = EDGE_CURVE ( 'NONE', #13042, #2286, #18662, .T. ) ;
#13226 = ORIENTED_EDGE ( 'NONE', *, *, #22, .T. ) ;
#13227 = EDGE_CURVE ( 'NONE', #7533, #13134, #7410, .T. ) ;
#13228 =( GEOMETRIC_REPRESENTATION_CONTEXT ( 3 ) GLOBAL_UNCERTAINTY_ASSIGNED_CONTEXT ( ( #4727 ) ) GLOBAL_UNIT_ASSIGNED_CONTEXT ( ( #6132, #11951, #16255 ) ) REPRESENTATION_CONTEXT ( 'NONE', 'WORKASPACE' ) );
#13229 = CARTESIAN_POINT ( 'NONE',  ( 55.85952145814821534, 6.938893903907228378E-15, 35.00000000000000000 ) ) ;
#13230 = AXIS2_PLACEMENT_3D ( 'NONE', #5925, #4491, #7174 ) ;
#13231 = CARTESIAN_POINT ( 'NONE',  ( -8.312069145893737243, -16.50572396040226053, 12.99038105676661026 ) ) ;
#13232 = CARTESIAN_POINT ( 'NONE',  ( -73.70149508017375695, -31.94019758230671258, -21.65063509461098334 ) ) ;
#13233 = DIRECTION ( 'NONE',  ( -0.1566598588826321192, 0.9876526153536342445, 7.798540720466730171E-17 ) ) ;
#13234 = DIRECTION ( 'NONE',  ( 1.000000000000000000, 0.000000000000000000, 0.000000000000000000 ) ) ;
#13235 = DIRECTION ( 'NONE',  ( -0.1566598588826321747, 0.9876526153536343555, 0.000000000000000000 ) ) ;
#13236 = CARTESIAN_POINT ( 'NONE',  ( -63.78533391645962780, -88.07278042982852639, -8.660254037844385522 ) ) ;
#13237 = DIRECTION ( 'NONE',  ( -0.1566598588826321747, 0.9876526153536343555, 0.000000000000000000 ) ) ;
#13238 = DIRECTION ( 'NONE',  ( -0.1566598588826321747, 0.9876526153536343555, 0.000000000000000000 ) ) ;
#13240 = ORIENTED_EDGE ( 'NONE', *, *, #51, .F. ) ;
#13239 = DIRECTION ( 'NONE',  ( -0.000000000000000000, -0.000000000000000000, -1.000000000000000000 ) ) ;
#13241 = VECTOR ( 'NONE', #2835, 1000.000000000000000 ) ;
#13242 = EDGE_LOOP ( 'NONE', ( #17658, #5222, #13801, #12277 ) ) ;
#13243 = CARTESIAN_POINT ( 'NONE',  ( -126.1404785418517918, 6.938893903907228378E-15, 2.500000000000000000 ) ) ;
#13244 = ORIENTED_EDGE ( 'NONE', *, *, #6879, .T. ) ;
#13245 = EDGE_CURVE ( 'NONE', #9271, #17419, #15264, .T. ) ;
#13246 = VERTEX_POINT ( 'NONE', #18255 ) ;
#13247 = DIRECTION ( 'NONE',  ( -0.9876526153536341335, -0.1566598588826327576, 0.000000000000000000 ) ) ;
#13248 = CIRCLE ( 'NONE', #12028, 1.500000000000000888 ) ;
#13249 = DIRECTION ( 'NONE',  ( -0.1566598588826321747, 0.9876526153536343555, 0.000000000000000000 ) ) ;
#13250 = AXIS2_PLACEMENT_3D ( 'NONE', #3623, #13762, #8199 ) ;
#13251 = EDGE_CURVE ( 'NONE', #983, #3927, #8517, .T. ) ;
#13252 = CARTESIAN_POINT ( 'NONE',  ( -9.464440072009985272, -79.45648819128378193, -17.32050807568878525 ) ) ;
#13253 = VERTEX_POINT ( 'NONE', #16597 ) ;
#13254 = AXIS2_PLACEMENT_3D ( 'NONE', #17927, #12179, #13505 ) ;
#13255 = CARTESIAN_POINT ( 'NONE',  ( -35.14340807120434818, -83.52964452223221770, 12.99038105676661203 ) ) ;
#13256 = ORIENTED_EDGE ( 'NONE', *, *, #18250, .F. ) ;
#13257 = FACE_BOUND ( 'NONE', #4865, .T. ) ;
#13258 = AXIS2_PLACEMENT_3D ( 'NONE', #2490, #12423, #18266 ) ;
#13259 = CARTESIAN_POINT ( 'NONE',  ( 0.000000000000000000, 0.000000000000000000, -37.00000000000000711 ) ) ;
#13260 = ORIENTED_EDGE ( 'NONE', *, *, #3328, .T. ) ;
#13261 = CARTESIAN_POINT ( 'NONE',  ( -76.95392591297100182, -27.39358415274517000, -8.660254037844380193 ) ) ;
#13262 = VECTOR ( 'NONE', #5624, 1000.000000000000227 ) ;
#13263 = AXIS2_PLACEMENT_3D ( 'NONE', #17728, #14763, #8801 ) ;
#13264 = CARTESIAN_POINT ( 'NONE',  ( -7.982961148979534016, -79.22149840295983836, -8.660254037844385522 ) ) ;
#13265 = CIRCLE ( 'NONE', #14492, 1.500000000000000888 ) ;
#13266 = VERTEX_POINT ( 'NONE', #3584 ) ;
#13267 = ORIENTED_EDGE ( 'NONE', *, *, #3347, .F. ) ;
#13268 = ORIENTED_EDGE ( 'NONE', *, *, #10970, .F. ) ;
#13269 = EDGE_LOOP ( 'NONE', ( #9647, #15374, #13226, #4881 ) ) ;
#13270 = CARTESIAN_POINT ( 'NONE',  ( 10.28861223506262412, -76.32329101363113466, 8.660254037844406838 ) ) ;
#13271 = VERTEX_POINT ( 'NONE', #7017 ) ;
#13272 = FACE_BOUND ( 'NONE', #2804, .T. ) ;
#13273 = CIRCLE ( 'NONE', #14214, 1.500000000000000888 ) ;
#13274 = CARTESIAN_POINT ( 'NONE',  ( -52.96079015774756726, -28.65034054577146705, -8.660254037844380193 ) ) ;
#13275 = ORIENTED_EDGE ( 'NONE', *, *, #18576, .T. ) ;
#13276 = EDGE_CURVE ( 'NONE', #6476, #11377, #10722, .T. ) ;
#13277 = LINE ( 'NONE', #17867, #11853 ) ;
#13278 = AXIS2_PLACEMENT_3D ( 'NONE', #10128, #6842, #18542 ) ;
#13279 = ORIENTED_EDGE ( 'NONE', *, *, #6533, .T. ) ;
#13280 = AXIS2_PLACEMENT_3D ( 'NONE', #8954, #13212, #12848 ) ;
#13281 = CIRCLE ( 'NONE', #1752, 1.500000000000000444 ) ;
#13282 = AXIS2_PLACEMENT_3D ( 'NONE', #18046, #6752, #18636 ) ;
#13283 = AXIS2_PLACEMENT_3D ( 'NONE', #13308, #342, #3251 ) ;
#13284 = EDGE_LOOP ( 'NONE', ( #17557, #16829, #15153, #18721 ) ) ;
#13285 = EDGE_CURVE ( 'NONE', #2423, #3127, #9825, .T. ) ;
#13286 = DIRECTION ( 'NONE',  ( -0.1566598588826321192, 0.9876526153536342445, 7.798540720466730171E-17 ) ) ;
#13287 = DIRECTION ( 'NONE',  ( -0.9876526153536341335, -0.1566598588826327021, 0.000000000000000000 ) ) ;
#13288 = CARTESIAN_POINT ( 'NONE',  ( -31.52190560670403841, -20.18723064414411894, 12.99038105676661736 ) ) ;
#13289 = DIRECTION ( 'NONE',  ( -0.1566598588826321192, 0.9876526153536342445, 7.798540720466730171E-17 ) ) ;
#13290 = AXIS2_PLACEMENT_3D ( 'NONE', #6435, #18008, #4967 ) ;
#13291 = LINE ( 'NONE', #10543, #16570 ) ;
#13292 = VERTEX_POINT ( 'NONE', #9391 ) ;
#13293 = VERTEX_POINT ( 'NONE', #15169 ) ;
#13294 = FACE_BOUND ( 'NONE', #9800, .T. ) ;
#13295 = DIRECTION ( 'NONE',  ( -0.000000000000000000, -0.000000000000000000, -1.000000000000000000 ) ) ;
#13296 = CIRCLE ( 'NONE', #5129, 1.499999999999999556 ) ;
#13297 = CARTESIAN_POINT ( 'NONE',  ( 0.5768043922889515285, -15.09578523045857601, -17.32050807568878170 ) ) ;
#13298 = DIRECTION ( 'NONE',  ( -0.1566598588826321192, 0.9876526153536342445, 7.798540720466731404E-17 ) ) ;
#13299 = ORIENTED_EDGE ( 'NONE', *, *, #15821, .F. ) ;
#13300 = APPLICATION_CONTEXT ( 'automotive_design' ) ;
#13301 = AXIS2_PLACEMENT_3D ( 'NONE', #1987, #12004, #7773 ) ;
#13302 = ORIENTED_EDGE ( 'NONE', *, *, #4285, .F. ) ;
#13303 = CYLINDRICAL_SURFACE ( 'NONE', #5186, 1.500000000000001554 ) ;
#13304 = AXIS2_PLACEMENT_3D ( 'NONE', #12772, #11332, #1413 ) ;
#13305 = EDGE_CURVE ( 'NONE', #5271, #17224, #11625, .T. ) ;
#13306 = CARTESIAN_POINT ( 'NONE',  ( -73.49714175923330117, -26.84527464665596241, 8.660254037844417496 ) ) ;
#13307 = EDGE_CURVE ( 'NONE', #2732, #14342, #14060, .T. ) ;
#13308 = CARTESIAN_POINT ( 'NONE',  ( -16.70711637639958269, -17.83733276090463349, -21.65063509461097979 ) ) ;
#13309 = DIRECTION ( 'NONE',  ( -1.000000000000000000, 0.000000000000000000, 0.000000000000000000 ) ) ;
#13310 = EDGE_CURVE ( 'NONE', #13701, #8275, #1323, .T. ) ;
#13311 = ORIENTED_EDGE ( 'NONE', *, *, #13101, .F. ) ;
#13312 = AXIS2_PLACEMENT_3D ( 'NONE', #5135, #1087, #12702 ) ;
#13313 = CARTESIAN_POINT ( 'NONE',  ( -0.9046745307415022808, -15.33077501878252136, 8.660254037844412167 ) ) ;
#13314 = AXIS2_PLACEMENT_3D ( 'NONE', #10742, #16660, #9532 ) ;
#13315 = CARTESIAN_POINT ( 'NONE',  ( -2.000000000000000000, 0.000000000000000000, -30.00000000000000000 ) ) ;
#13316 = DIRECTION ( 'NONE',  ( -0.9876526153536341335, -0.1566598588826327021, 0.000000000000000000 ) ) ;
#13317 = DIRECTION ( 'NONE',  ( -0.1566598588826321192, 0.9876526153536342445, 7.798540720466730171E-17 ) ) ;
#13318 = VERTEX_POINT ( 'NONE', #12299 ) ;
#13319 = DIRECTION ( 'NONE',  ( 0.000000000000000000, 0.000000000000000000, 1.000000000000000000 ) ) ;
#13320 = ORIENTED_EDGE ( 'NONE', *, *, #9097, .F. ) ;
#13321 = AXIS2_PLACEMENT_3D ( 'NONE', #5281, #13693, #10949 ) ;
#13322 = AXIS2_PLACEMENT_3D ( 'NONE', #2041, #4688, #2140 ) ;
#13323 = ORIENTED_EDGE ( 'NONE', *, *, #1970, .F. ) ;
#13324 = ORIENTED_EDGE ( 'NONE', *, *, #12501, .F. ) ;
#13325 = CIRCLE ( 'NONE', #1257, 1.500000000000001332 ) ;
#13326 = DIRECTION ( 'NONE',  ( 0.000000000000000000, 0.000000000000000000, 1.000000000000000000 ) ) ;
#13327 = AXIS2_PLACEMENT_3D ( 'NONE', #4110, #2526, #8313 ) ;
#13328 = EDGE_CURVE ( 'NONE', #15786, #16387, #2568, .T. ) ;
#13329 = CARTESIAN_POINT ( 'NONE',  ( 11.59211860341528855, 6.314490184041240184, -20.00000000000000355 ) ) ;
#13330 = CYLINDRICAL_SURFACE ( 'NONE', #13110, 1.500000000000001554 ) ;
#13331 = ORIENTED_EDGE ( 'NONE', *, *, #174, .T. ) ;
#13332 = CYLINDRICAL_SURFACE ( 'NONE', #12421, 1.500000000000001554 ) ;
#13333 = DIRECTION ( 'NONE',  ( -0.1566598588826321192, 0.9876526153536342445, 7.798540720466731404E-17 ) ) ;
#13334 =( LENGTH_UNIT ( ) NAMED_UNIT ( * ) SI_UNIT ( .MILLI., .METRE. ) );
#13335 = ORIENTED_EDGE ( 'NONE', *, *, #15064, .F. ) ;
#13336 = AXIS2_PLACEMENT_3D ( 'NONE', #1126, #7182, #15689 ) ;
#13337 = EDGE_CURVE ( 'NONE', #8644, #9857, #1660, .T. ) ;
#13338 = LINE ( 'NONE', #17363, #571 ) ;
#13339 = ORIENTED_EDGE ( 'NONE', *, *, #9297, .T. ) ;
#13340 = CIRCLE ( 'NONE', #8521, 1.500000000000000888 ) ;
#13341 = CARTESIAN_POINT ( 'NONE',  ( -1.892327146095121204, -15.48743487766515337, -12.99038105676658361 ) ) ;
#13342 = EDGE_CURVE ( 'NONE', #16721, #518, #15205, .T. ) ;
#13343 = CARTESIAN_POINT ( 'NONE',  ( -81.73462711737164454, 33.01666666666666572, -35.00000000000000000 ) ) ;
#13344 = EDGE_LOOP ( 'NONE', ( #10193, #13176 ) ) ;
#13345 = CIRCLE ( 'NONE', #11228, 2.000000000000000000 ) ;
#13347 = EDGE_LOOP ( 'NONE', ( #4508, #12814 ) ) ;
#13346 = LINE ( 'NONE', #561, #18184 ) ;
#13348 = AXIS2_PLACEMENT_3D ( 'NONE', #3798, #18284, #2217 ) ;
#13349 = EDGE_LOOP ( 'NONE', ( #17399, #3816 ) ) ;
#13350 = CARTESIAN_POINT ( 'NONE',  ( -8.312069145893737243, -16.50572396040226053, -4.330127018922183879 ) ) ;
#13351 = ORIENTED_EDGE ( 'NONE', *, *, #17803, .T. ) ;
#13352 = ORIENTED_EDGE ( 'NONE', *, *, #2238, .F. ) ;
#13353 = AXIS2_PLACEMENT_3D ( 'NONE', #18624, #2832, #15715 ) ;
#13354 = CYLINDRICAL_SURFACE ( 'NONE', #6577, 1.500000000000000888 ) ;
#13355 = CARTESIAN_POINT ( 'NONE',  ( -54.73174206751431115, -23.86873732788597025, 21.65063509461101887 ) ) ;
#13356 = VECTOR ( 'NONE', #8623, 1000.000000000000000 ) ;
#13357 = CARTESIAN_POINT ( 'NONE',  ( -60.36818477289977380, -29.82528948739119556, 21.65063509461101887 ) ) ;
#13358 = CARTESIAN_POINT ( 'NONE',  ( -70.24471092643608472, -31.39188807621751209, 12.99038105676661736 ) ) ;
#13359 = DIRECTION ( 'NONE',  ( -0.1566598588826321192, 0.9876526153536342445, 7.798540720466730171E-17 ) ) ;
#13360 = DIRECTION ( 'NONE',  ( -0.1566598588826321192, 0.9876526153536342445, 7.798540720466731404E-17 ) ) ;
#13361 = ORIENTED_EDGE ( 'NONE', *, *, #3645, .F. ) ;
#13362 = EDGE_CURVE ( 'NONE', #8019, #5828, #12845, .T. ) ;
#13363 = VECTOR ( 'NONE', #15469, 1000.000000000000000 ) ;
#13364 = EDGE_CURVE ( 'NONE', #931, #10329, #1593, .T. ) ;
#13365 = SURFACE_SIDE_STYLE ('',( #14613 ) ) ;
#13366 = ORIENTED_EDGE ( 'NONE', *, *, #12332, .F. ) ;
#13367 = CARTESIAN_POINT ( 'NONE',  ( -34.15575545585073058, -83.37298466334958391, 17.32050807568881368 ) ) ;
#13368 = CARTESIAN_POINT ( 'NONE',  ( -67.24211807019732134, -88.62108993591775175, 8.660254037844412167 ) ) ;
#13369 = CIRCLE ( 'NONE', #13077, 1.500000000000000888 ) ;
#13370 = ADVANCED_FACE ( 'NONE', ( #7192 ), #3085, .F. ) ;
#13371 = ORIENTED_EDGE ( 'NONE', *, *, #10708, .F. ) ;
#13372 = EDGE_LOOP ( 'NONE', ( #18539, #4701, #9636, #2019 ) ) ;
#13373 = ORIENTED_EDGE ( 'NONE', *, *, #10660, .F. ) ;
#13374 = ORIENTED_EDGE ( 'NONE', *, *, #7474, .T. ) ;
#13375 = CYLINDRICAL_SURFACE ( 'NONE', #10462, 1.500000000000001554 ) ;
#13376 = ORIENTED_EDGE ( 'NONE', *, *, #10351, .T. ) ;
#13377 = FACE_BOUND ( 'NONE', #14794, .T. ) ;
#13378 = VECTOR ( 'NONE', #5982, 1000.000000000000000 ) ;
#13379 = FACE_OUTER_BOUND ( 'NONE', #17048, .T. ) ;
#13380 = ORIENTED_EDGE ( 'NONE', *, *, #7889, .F. ) ;
#13381 = MECHANICAL_DESIGN_GEOMETRIC_PRESENTATION_REPRESENTATION (  '', ( #4001 ), #3686 ) ;
#13382 = ORIENTED_EDGE ( 'NONE', *, *, #7970, .F. ) ;
#13383 = CYLINDRICAL_SURFACE ( 'NONE', #10883, 1.500000000000001554 ) ;
#13384 = DIRECTION ( 'NONE',  ( -0.9876526153536341335, -0.1566598588826327576, 0.000000000000000000 ) ) ;
#13385 = FACE_OUTER_BOUND ( 'NONE', #8860, .T. ) ;
#13386 = DIRECTION ( 'NONE',  ( -0.1566598588826321747, 0.9876526153536343555, 0.000000000000000000 ) ) ;
#13387 = ORIENTED_EDGE ( 'NONE', *, *, #2552, .T. ) ;
#13388 = ORIENTED_EDGE ( 'NONE', *, *, #17570, .T. ) ;
#13389 = CYLINDRICAL_SURFACE ( 'NONE', #14776, 1.500000000000001554 ) ;
#13390 = ADVANCED_FACE ( 'NONE', ( #14383 ), #17716, .F. ) ;
#13391 = CARTESIAN_POINT ( 'NONE',  ( 2.200000000000000178, 2.694222958124177006E-16, 20.00000000000000000 ) ) ;
#13392 = CIRCLE ( 'NONE', #16448, 1.499999999999999556 ) ;
#13393 = EDGE_LOOP ( 'NONE', ( #5036, #8011 ) ) ;
#13394 = DIRECTION ( 'NONE',  ( -0.1566598588826321747, 0.9876526153536343555, 0.000000000000000000 ) ) ;
#13395 = EDGE_CURVE ( 'NONE', #2096, #3287, #2892, .T. ) ;
#13396 = LINE ( 'NONE', #7539, #17616 ) ;
#13397 = CARTESIAN_POINT ( 'NONE',  ( -24.11451099155181055, -19.01228170252437621, 1.908195823574487804E-14 ) ) ;
#13398 = FACE_OUTER_BOUND ( 'NONE', #17966, .T. ) ;
#13399 = AXIS2_PLACEMENT_3D ( 'NONE', #4614, #17818, #11887 ) ;
#13400 = CARTESIAN_POINT ( 'NONE',  ( -129.1404785418517918, -2.850701963179328668, 9.951701414186818625E-16 ) ) ;
#13401 = SURFACE_STYLE_FILL_AREA ( #11875 ) ;
#13402 = DIRECTION ( 'NONE',  ( 8.693966348389027220E-17, -1.991237296706374949E-16, 1.000000000000000000 ) ) ;
#13403 = CARTESIAN_POINT ( 'NONE',  ( -49.79347899074618056, -23.08543803347280488, 4.330127018922218518 ) ) ;
#13404 = ORIENTED_EDGE ( 'NONE', *, *, #7520, .F. ) ;
#13405 = ORIENTED_EDGE ( 'NONE', *, *, #14726, .T. ) ;
#13406 = PLANE ( 'NONE',  #4256 ) ;
#13407 = ORIENTED_EDGE ( 'NONE', *, *, #12728, .F. ) ;
#13408 = EDGE_CURVE ( 'NONE', #10248, #11883, #1969, .T. ) ;
#13409 = ORIENTED_EDGE ( 'NONE', *, *, #16765, .F. ) ;
#13410 = VERTEX_POINT ( 'NONE', #2819 ) ;
#13411 = EDGE_CURVE ( 'NONE', #9589, #11831, #9850, .T. ) ;
#13412 = AXIS2_PLACEMENT_3D ( 'NONE', #18217, #742, #6523 ) ;
#13413 = DIRECTION ( 'NONE',  ( -0.9876526153536341335, -0.1566598588826327021, 0.000000000000000000 ) ) ;
#13414 = CARTESIAN_POINT ( 'NONE',  ( -52.92115514756970640, -86.34952198211959740, 21.65063509461101532 ) ) ;
#13415 = DIRECTION ( 'NONE',  ( 0.000000000000000000, 0.000000000000000000, 1.000000000000000000 ) ) ;
#13416 = CARTESIAN_POINT ( 'NONE',  ( -62.63296299034339398, -25.12201619894700144, -21.65063509461098334 ) ) ;
#13417 = DIRECTION ( 'NONE',  ( -0.1566598588826321747, 0.9876526153536343555, 0.000000000000000000 ) ) ;
#13418 = CARTESIAN_POINT ( 'NONE',  ( -81.87192997736543987, 3.395211045985502274, -2.500000000000000000 ) ) ;
#13419 = ORIENTED_EDGE ( 'NONE', *, *, #8952, .F. ) ;
#13420 = DIRECTION ( 'NONE',  ( -0.9876526153536336894, -0.1566598588826349503, 0.000000000000000000 ) ) ;
#13421 = DIRECTION ( 'NONE',  ( -0.9876526153536336894, -0.1566598588826349503, 0.000000000000000000 ) ) ;
#13422 = ORIENTED_EDGE ( 'NONE', *, *, #8473, .F. ) ;
#13423 = DIRECTION ( 'NONE',  ( 0.000000000000000000, 0.000000000000000000, 1.000000000000000000 ) ) ;
#13424 = EDGE_CURVE ( 'NONE', #3317, #12090, #15895, .T. ) ;
#13426 = VERTEX_POINT ( 'NONE', #14467 ) ;
#13425 = CYLINDRICAL_SURFACE ( 'NONE', #3276, 1.500000000000001554 ) ;
#13427 = EDGE_CURVE ( 'NONE', #14148, #1617, #1498, .T. ) ;
#13428 = DIRECTION ( 'NONE',  ( 1.000000000000000000, 0.000000000000000000, 0.000000000000000000 ) ) ;
#13429 = ADVANCED_FACE ( 'NONE', ( #17522 ), #10288, .F. ) ;
#13430 = VERTEX_POINT ( 'NONE', #10187 ) ;
#13431 = ORIENTED_EDGE ( 'NONE', *, *, #6857, .T. ) ;
#13432 = CYLINDRICAL_SURFACE ( 'NONE', #5356, 1.500000000000001554 ) ;
#13433 = LINE ( 'NONE', #14962, #5522 ) ;
#13434 = ORIENTED_EDGE ( 'NONE', *, *, #359, .T. ) ;
#13435 = FACE_OUTER_BOUND ( 'NONE', #13153, .T. ) ;
#13436 = VERTEX_POINT ( 'NONE', #5859 ) ;
#13437 = DIRECTION ( 'NONE',  ( 0.000000000000000000, 0.000000000000000000, 1.000000000000000000 ) ) ;
#13438 = CYLINDRICAL_SURFACE ( 'NONE', #16714, 1.500000000000001554 ) ;
#13439 = FACE_OUTER_BOUND ( 'NONE', #14220, .T. ) ;
#13440 = AXIS2_PLACEMENT_3D ( 'NONE', #13721, #5483, #5004 ) ;
#13441 = DIRECTION ( 'NONE',  ( -0.000000000000000000, -0.000000000000000000, -1.000000000000000000 ) ) ;
#13442 = DIRECTION ( 'NONE',  ( 0.000000000000000000, 0.000000000000000000, 1.000000000000000000 ) ) ;
#13443 = ORIENTED_EDGE ( 'NONE', *, *, #12055, .T. ) ;
#13444 = DIRECTION ( 'NONE',  ( -0.1566598588826321747, 0.9876526153536343555, 0.000000000000000000 ) ) ;
#13445 = ORIENTED_EDGE ( 'NONE', *, *, #18250, .T. ) ;
#13446 = CARTESIAN_POINT ( 'NONE',  ( -176.1167811578620501, -139.6880237571007513, 2.500000000000000000 ) ) ;
#13447 = DIRECTION ( 'NONE',  ( -0.1566598588826321192, 0.9876526153536342445, 7.798540720466731404E-17 ) ) ;
#13448 = ORIENTED_EDGE ( 'NONE', *, *, #5885, .T. ) ;
#13449 = EDGE_LOOP ( 'NONE', ( #12180, #12592, #7244, #11757 ) ) ;
#13450 = ORIENTED_EDGE ( 'NONE', *, *, #1465, .F. ) ;
#13451 = ORIENTED_EDGE ( 'NONE', *, *, #8242, .T. ) ;
#13452 = CARTESIAN_POINT ( 'NONE',  ( -24.27922930231443743, -81.80638607452327449, 17.32050807568881368 ) ) ;
#13453 = ORIENTED_EDGE ( 'NONE', *, *, #17570, .F. ) ;
#13454 = VERTEX_POINT ( 'NONE', #11605 ) ;
#13455 = CIRCLE ( 'NONE', #17433, 1.499999999999999556 ) ;
#13456 = FACE_BOUND ( 'NONE', #13689, .T. ) ;
#13457 = ADVANCED_FACE ( 'NONE', ( #349 ), #17427, .F. ) ;
#13458 = ADVANCED_FACE ( 'NONE', ( #1405 ), #2986, .F. ) ;
#13459 = DIRECTION ( 'NONE',  ( -0.9876526153536341335, -0.1566598588826327021, 0.000000000000000000 ) ) ;
#13460 = VERTEX_POINT ( 'NONE', #8780 ) ;
#13461 = EDGE_LOOP ( 'NONE', ( #15822, #5240 ) ) ;
#13462 = DIRECTION ( 'NONE',  ( -0.1566598588826321747, 0.9876526153536343555, 0.000000000000000000 ) ) ;
#13463 = FACE_BOUND ( 'NONE', #3094, .T. ) ;
#13464 = CARTESIAN_POINT ( 'NONE',  ( -84.16561914167408531, -33.59999999999994458, 30.00000000000000000 ) ) ;
#13465 = VECTOR ( 'NONE', #3148, 1000.000000000000114 ) ;
#13466 = DIRECTION ( 'NONE',  ( -0.9876526153536344665, -0.1566598588826304539, 0.000000000000000000 ) ) ;
#13467 = LINE ( 'NONE', #4937, #15906 ) ;
#13468 = DIRECTION ( 'NONE',  ( -0.1566598588826321747, 0.9876526153536343555, 0.000000000000000000 ) ) ;
#13469 = ORIENTED_EDGE ( 'NONE', *, *, #1172, .T. ) ;
#13470 = ORIENTED_EDGE ( 'NONE', *, *, #18448, .T. ) ;
#13471 = CARTESIAN_POINT ( 'NONE',  ( -85.13801595139511846, 33.83333333333333570, 30.00000000000005329 ) ) ;
#13472 = FACE_OUTER_BOUND ( 'NONE', #15564, .T. ) ;
#13473 = VERTEX_POINT ( 'NONE', #245 ) ;
#13474 = EDGE_LOOP ( 'NONE', ( #164, #1861 ) ) ;
#13475 = CARTESIAN_POINT ( 'NONE',  ( -45.01993422474066620, -85.09624311105851291, -12.99038105676658539 ) ) ;
#13476 = EDGE_LOOP ( 'NONE', ( #15666, #6469 ) ) ;
#13477 = FACE_OUTER_BOUND ( 'NONE', #11195, .T. ) ;
#13478 = ADVANCED_FACE ( 'NONE', ( #18781 ), #6032, .T. ) ;
#13479 = DIRECTION ( 'NONE',  ( 1.000000000000000000, 0.000000000000000000, 0.000000000000000000 ) ) ;
#13480 = ORIENTED_EDGE ( 'NONE', *, *, #8911, .F. ) ;
#13481 = AXIS2_PLACEMENT_3D ( 'NONE', #780, #18150, #9490 ) ;
#13482 = DIRECTION ( 'NONE',  ( 0.000000000000000000, 0.000000000000000000, 1.000000000000000000 ) ) ;
#13483 = EDGE_CURVE ( 'NONE', #12253, #15050, #767, .T. ) ;
#13484 = DIRECTION ( 'NONE',  ( -0.1566598588826321192, 0.9876526153536342445, 7.798540720466730171E-17 ) ) ;
#13485 = DIRECTION ( 'NONE',  ( -0.1566598588826321192, 0.9876526153536342445, 7.798540720466731404E-17 ) ) ;
#13486 = EDGE_LOOP ( 'NONE', ( #7365, #13073 ) ) ;
#13487 = ORIENTED_EDGE ( 'NONE', *, *, #16832, .F. ) ;
#13488 = DIRECTION ( 'NONE',  ( -0.1566598588826321192, 0.9876526153536342445, 7.798540720466730171E-17 ) ) ;
#13489 = CIRCLE ( 'NONE', #5019, 1.500000000000001332 ) ;
#13490 = ORIENTED_EDGE ( 'NONE', *, *, #10526, .T. ) ;
#13491 = DIRECTION ( 'NONE',  ( -0.9876526153536341335, -0.1566598588826327021, 0.000000000000000000 ) ) ;
#13492 = ORIENTED_EDGE ( 'NONE', *, *, #4888, .F. ) ;
#13493 = ORIENTED_EDGE ( 'NONE', *, *, #7664, .T. ) ;
#13494 = AXIS2_PLACEMENT_3D ( 'NONE', #11266, #11442, #15622 ) ;
#13495 = AXIS2_PLACEMENT_3D ( 'NONE', #11545, #2926, #4163 ) ;
#13496 = DIRECTION ( 'NONE',  ( -0.9876526153536336894, -0.1566598588826349503, 0.000000000000000000 ) ) ;
#13497 = CARTESIAN_POINT ( 'NONE',  ( -61.35583738825340561, -29.98194934627382224, -8.660254037844380193 ) ) ;
#13498 = ORIENTED_EDGE ( 'NONE', *, *, #16533, .F. ) ;
#13499 = DIRECTION ( 'NONE',  ( -0.1566598588826321192, 0.9876526153536342445, 7.798540720466730171E-17 ) ) ;
#13500 = CARTESIAN_POINT ( 'NONE',  ( -81.73462711737164454, 33.01666666666666572, 30.00000000000000000 ) ) ;
#13501 = EDGE_CURVE ( 'NONE', #8368, #17125, #11511, .T. ) ;
#13502 = DIRECTION ( 'NONE',  ( -0.9876526153536341335, -0.1566598588826327021, 0.000000000000000000 ) ) ;
#13503 = CIRCLE ( 'NONE', #12902, 3.000000000000000000 ) ;
#13504 = CARTESIAN_POINT ( 'NONE',  ( -29.75095369693726255, -24.96883386202961574, -17.32050807568878170 ) ) ;
#13505 = DIRECTION ( 'NONE',  ( -0.9876526153536344665, -0.1566598588826304539, 0.000000000000000000 ) ) ;
#13506 = AXIS2_PLACEMENT_3D ( 'NONE', #11053, #956, #1974 ) ;
#13507 = B_SPLINE_CURVE_WITH_KNOTS ( 'NONE', 3,
 ( #1487, #7275, #15971, #8767 ),
 .UNSPECIFIED., .F., .F.,
 ( 4, 4 ),
 ( 0.000000000000000000, 0.003000475340473870295 ),
 .UNSPECIFIED. ) ;
#13508 = CARTESIAN_POINT ( 'NONE',  ( -26.58364252993588650, -19.40393134973095712, 4.330127018922218518 ) ) ;
#13509 = CARTESIAN_POINT ( 'NONE',  ( -3.373806069125576901, -15.72242466598909871, 12.99038105676661026 ) ) ;
#13510 = AXIS2_PLACEMENT_3D ( 'NONE', #1681, #256, #6150 ) ;
#13511 = EDGE_CURVE ( 'NONE', #17176, #6871, #6597, .T. ) ;
#13512 = CYLINDRICAL_SURFACE ( 'NONE', #553, 1.500000000000001554 ) ;
#13513 = CARTESIAN_POINT ( 'NONE',  ( -20.86208015875458344, -23.55889513208593655, -4.330127018922181215 ) ) ;
#13515 = ORIENTED_EDGE ( 'NONE', *, *, #128, .F. ) ;
#13514 = FACE_OUTER_BOUND ( 'NONE', #5434, .T. ) ;
#13516 = DIRECTION ( 'NONE',  ( -0.9876526153536341335, -0.1566598588826327021, 0.000000000000000000 ) ) ;
#13517 = AXIS2_PLACEMENT_3D ( 'NONE', #11135, #8223, #17057 ) ;
#13518 = VERTEX_POINT ( 'NONE', #3258 ) ;
#13519 = AXIS2_PLACEMENT_3D ( 'NONE', #1746, #13298, #17789 ) ;
#13520 = VERTEX_POINT ( 'NONE', #11956 ) ;
#13521 = CARTESIAN_POINT ( 'NONE',  ( -129.1404785418517918, -2.850701963179328668, 9.951701414186818625E-16 ) ) ;
#13522 = EDGE_CURVE ( 'NONE', #10673, #14246, #7732, .T. ) ;
#13523 = LINE ( 'NONE', #16409, #15495 ) ;
#13524 = AXIS2_PLACEMENT_3D ( 'NONE', #3840, #8325, #18517 ) ;
#13525 = LINE ( 'NONE', #574, #10675 ) ;
#13526 = DIRECTION ( 'NONE',  ( 0.000000000000000000, 0.000000000000000000, 1.000000000000000000 ) ) ;
#13527 = EDGE_LOOP ( 'NONE', ( #2679, #6796, #539, #415 ) ) ;
#13528 = CARTESIAN_POINT ( 'NONE',  ( -79.91688375903190433, -27.86356372939307136, 17.32050807568881723 ) ) ;
#13529 = ADVANCED_FACE ( 'NONE', ( #818 ), #5172, .F. ) ;
#13530 = ADVANCED_FACE ( 'NONE', ( #13589 ), #3441, .F. ) ;
#13531 = CARTESIAN_POINT ( 'NONE',  ( -67.77557938805200877, -31.00023842901093118, 1.869203119972154228E-14 ) ) ;
#13532 = DIRECTION ( 'NONE',  ( -0.9876526153536341335, -0.1566598588826327021, 0.000000000000000000 ) ) ;
#13533 = DIRECTION ( 'NONE',  ( -0.9876526153536341335, -0.1566598588826330907, 0.000000000000000000 ) ) ;
#13534 = EDGE_LOOP ( 'NONE', ( #4838, #12224 ) ) ;
#13535 = FACE_BOUND ( 'NONE', #15381, .T. ) ;
#13536 = CIRCLE ( 'NONE', #17815, 150.0000000000000000 ) ;
#13537 = EDGE_CURVE ( 'NONE', #12885, #294, #2263, .T. ) ;
#13538 = FILL_AREA_STYLE ('',( #15251 ) ) ;
#13539 = EDGE_LOOP ( 'NONE', ( #4528, #4751, #18679, #5574 ) ) ;
#13540 = LINE ( 'NONE', #12010, #4053 ) ;
#13541 = DIRECTION ( 'NONE',  ( 0.000000000000000000, 0.000000000000000000, 1.000000000000000000 ) ) ;
#13542 = VECTOR ( 'NONE', #12559, 1000.000000000000000 ) ;
#13543 = ORIENTED_EDGE ( 'NONE', *, *, #131, .F. ) ;
#13544 = ORIENTED_EDGE ( 'NONE', *, *, #17175, .F. ) ;
#13545 = ORIENTED_EDGE ( 'NONE', *, *, #12119, .T. ) ;
#13546 = DIRECTION ( 'NONE',  ( -0.1566598588826321192, 0.9876526153536342445, 7.798540720466730171E-17 ) ) ;
#13547 = CIRCLE ( 'NONE', #4787, 2.000000000000000000 ) ;
#13548 = ORIENTED_EDGE ( 'NONE', *, *, #16091, .F. ) ;
#13549 = FACE_BOUND ( 'NONE', #2042, .T. ) ;
#13550 = AXIS2_PLACEMENT_3D ( 'NONE', #10392, #4797, #18014 ) ;
#13551 = DIRECTION ( 'NONE',  ( -0.1566598588826321192, 0.9876526153536342445, 7.798540720466730171E-17 ) ) ;
#13552 = ORIENTED_EDGE ( 'NONE', *, *, #3847, .F. ) ;
#13553 = EDGE_CURVE ( 'NONE', #15511, #16506, #17908, .T. ) ;
#13554 = ADVANCED_FACE ( 'NONE', ( #1860 ), #17805, .F. ) ;
#13555 = ORIENTED_EDGE ( 'NONE', *, *, #7206, .F. ) ;
#13556 = CIRCLE ( 'NONE', #251, 1.500000000000000888 ) ;
#13557 = CIRCLE ( 'NONE', #12652, 1.500000000000000888 ) ;
#13558 = CARTESIAN_POINT ( 'NONE',  ( -38.92930022185625205, -21.36217958576384746, -8.660254037844380193 ) ) ;
#13559 = AXIS2_PLACEMENT_3D ( 'NONE', #5184, #646, #7936 ) ;
#13560 = EDGE_LOOP ( 'NONE', ( #14729, #7143, #6203, #3888 ) ) ;
#13561 = CARTESIAN_POINT ( 'NONE',  ( -1.109027851681966492, -20.42569795443330349, 12.99038105676661026 ) ) ;
#13562 = EDGE_CURVE ( 'NONE', #2420, #15025, #16824, .T. ) ;
#13563 = EDGE_CURVE ( 'NONE', #16131, #5990, #7651, .T. ) ;
#13564 = EDGE_CURVE ( 'NONE', #7429, #12177, #6226, .T. ) ;
#13565 = DIRECTION ( 'NONE',  ( -0.1566598588826321192, 0.9876526153536342445, 7.798540720466731404E-17 ) ) ;
#13566 = CARTESIAN_POINT ( 'NONE',  ( 0.000000000000000000, 0.000000000000000000, -22.00000000000000711 ) ) ;
#13567 = ORIENTED_EDGE ( 'NONE', *, *, #8014, .F. ) ;
#13568 = VERTEX_POINT ( 'NONE', #10664 ) ;
#13569 = CARTESIAN_POINT ( 'NONE',  ( -68.72359699322777260, -88.85607972424169532, 17.32050807568881368 ) ) ;
#13570 = CARTESIAN_POINT ( 'NONE',  ( -45.51376053241748565, -85.17457304049985112, 1.424741226644455312E-14 ) ) ;
#13571 = DIRECTION ( 'NONE',  ( -0.9876526153536336894, -0.1566598588826349503, 0.000000000000000000 ) ) ;
#13572 = DIRECTION ( 'NONE',  ( -0.1566598588826321192, 0.9876526153536342445, 7.798540720466731404E-17 ) ) ;
#13573 = AXIS2_PLACEMENT_3D ( 'NONE', #17951, #13165, #13532 ) ;
#13574 = AXIS2_PLACEMENT_3D ( 'NONE', #7697, #200, #13541 ) ;
#13575 = VERTEX_POINT ( 'NONE', #15018 ) ;
#13576 = CARTESIAN_POINT ( 'NONE',  ( -24.31886431249228053, -24.10720463817513703, 4.330127018922217630 ) ) ;
#13577 = CIRCLE ( 'NONE', #13280, 1.500000000000000888 ) ;
#13578 = ORIENTED_EDGE ( 'NONE', *, *, #3267, .F. ) ;
#13579 = CIRCLE ( 'NONE', #12667, 1.500000000000000888 ) ;
#13580 = DIRECTION ( 'NONE',  ( -0.9876526153536336894, -0.1566598588826349503, 0.000000000000000000 ) ) ;
#13581 = DIRECTION ( 'NONE',  ( -0.1566598588826321192, 0.9876526153536342445, 7.798540720466730171E-17 ) ) ;
#13582 = CARTESIAN_POINT ( 'NONE',  ( -51.97313754239394257, -28.49368068688882971, -12.99038105676658006 ) ) ;
#13583 = SURFACE_SIDE_STYLE ('',( #7646 ) ) ;
#13584 = CIRCLE ( 'NONE', #286, 145.0000000000000284 ) ;
#13585 = DIRECTION ( 'NONE',  ( 0.1856185419698760941, -0.9826218788918640312, 0.000000000000000000 ) ) ;
#13587 = CYLINDRICAL_SURFACE ( 'NONE', #18429, 2.200000000000000178 ) ;
#13586 = CIRCLE ( 'NONE', #7857, 1.500000000000000000 ) ;
#13588 = ADVANCED_FACE ( 'NONE', ( #4782 ), #6425, .F. ) ;
#13589 = FACE_OUTER_BOUND ( 'NONE', #13269, .T. ) ;
#13590 = AXIS2_PLACEMENT_3D ( 'NONE', #11874, #16650, #17713 ) ;
#13591 = EDGE_LOOP ( 'NONE', ( #15214, #38, #5064, #3539 ) ) ;
#13592 = ORIENTED_EDGE ( 'NONE', *, *, #757, .T. ) ;
#13593 = DIRECTION ( 'NONE',  ( 0.000000000000000000, 0.000000000000000000, 1.000000000000000000 ) ) ;
#13594 = ADVANCED_FACE ( 'NONE', ( #536 ), #16462, .T. ) ;
#13595 = CIRCLE ( 'NONE', #18511, 1.499999999999999556 ) ;
#13596 = VECTOR ( 'NONE', #4170, 1000.000000000000000 ) ;
#13597 = ORIENTED_EDGE ( 'NONE', *, *, #17202, .T. ) ;
#13598 = EDGE_CURVE ( 'NONE', #7971, #794, #13455, .T. ) ;
#13599 = DIRECTION ( 'NONE',  ( -0.9876526153536341335, -0.1566598588826327576, 0.000000000000000000 ) ) ;
#13600 = VERTEX_POINT ( 'NONE', #13771 ) ;
#13601 = AXIS2_PLACEMENT_3D ( 'NONE', #222, #3233, #4853 ) ;
#13602 = CARTESIAN_POINT ( 'NONE',  ( -2.096680467035594297, -20.58235781331593017, 1.540628126764003082E-14 ) ) ;
#13603 = LINE ( 'NONE', #9640, #17795 ) ;
#13604 = AXIS2_PLACEMENT_3D ( 'NONE', #2799, #8586, #14357 ) ;
#13605 = CARTESIAN_POINT ( 'NONE',  ( -62.79768130110601021, -87.91612057094590682, -12.99038105676658539 ) ) ;
#13606 = DIRECTION ( 'NONE',  ( 0.9868632313631133801, -0.1615579233078772714, 0.000000000000000000 ) ) ;
#13607 = ORIENTED_EDGE ( 'NONE', *, *, #17809, .F. ) ;
#13608 = DIRECTION ( 'NONE',  ( -0.1566598588826321192, 0.9876526153536342445, 7.798540720466730171E-17 ) ) ;
#13609 = VECTOR ( 'NONE', #12475, 1000.000000000000000 ) ;
#13610 = DIRECTION ( 'NONE',  ( -0.1615579233078775490, 0.9868632313631133801, 0.000000000000000000 ) ) ;
#13611 = CARTESIAN_POINT ( 'NONE',  ( 0.000000000000000000, 0.000000000000000000, 0.000000000000000000 ) ) ;
#13612 = CARTESIAN_POINT ( 'NONE',  ( -49.95819730150879678, -85.87954240547168183, 12.99038105676661203 ) ) ;
#13613 = DIRECTION ( 'NONE',  ( -0.9876526153536336894, -0.1566598588826350336, 0.000000000000000000 ) ) ;
#13614 = AXIS2_PLACEMENT_3D ( 'NONE', #7295, #8018, #10843 ) ;
#13615 = FACE_OUTER_BOUND ( 'NONE', #5744, .T. ) ;
#13616 = DIRECTION ( 'NONE',  ( -0.1566598588826321747, 0.9876526153536343555, 0.000000000000000000 ) ) ;
#13617 = DIRECTION ( 'NONE',  ( -0.9876526153536336894, -0.1566598588826350336, 0.000000000000000000 ) ) ;
#13619 = ORIENTED_EDGE ( 'NONE', *, *, #18600, .F. ) ;
#13618 = DIRECTION ( 'NONE',  ( -0.1566598588826321747, 0.9876526153536343555, 0.000000000000000000 ) ) ;
#13620 = ORIENTED_EDGE ( 'NONE', *, *, #12119, .F. ) ;
#13621 = VECTOR ( 'NONE', #28, 1000.000000000000000 ) ;
#13622 = CARTESIAN_POINT ( 'NONE',  ( 73.09088021254186174, 1.387778780781445676E-14, 25.00000000000000000 ) ) ;
#13623 = EDGE_CURVE ( 'NONE', #3731, #5983, #11333, .T. ) ;
#13624 = AXIS2_PLACEMENT_3D ( 'NONE', #11125, #9446, #13599 ) ;
#13625 = CARTESIAN_POINT ( 'NONE',  ( -7.528769851480577202, -21.44398703717040888, 21.65063509461101177 ) ) ;
#13626 = ORIENTED_EDGE ( 'NONE', *, *, #14968, .F. ) ;
#13627 = ORIENTED_EDGE ( 'NONE', *, *, #14355, .T. ) ;
#13628 = CARTESIAN_POINT ( 'NONE',  ( -3.382878129548355872, -13.70423786865302063, -19.99999999999998934 ) ) ;
#13629 = EDGE_CURVE ( 'NONE', #8364, #16586, #16509, .T. ) ;
#13630 = ORIENTED_EDGE ( 'NONE', *, *, #10213, .T. ) ;
#13631 = CIRCLE ( 'NONE', #17302, 1.499999999999999556 ) ;
#13632 = DIRECTION ( 'NONE',  ( -0.1566598588826321192, 0.9876526153536342445, 7.798540720466730171E-17 ) ) ;
#13633 = CIRCLE ( 'NONE', #17618, 1.500000000000001332 ) ;
#13634 = CARTESIAN_POINT ( 'NONE',  ( -2.000000000000000000, 2.449293598294706414E-16, 30.00000000000000000 ) ) ;
#13635 = DIRECTION ( 'NONE',  ( -0.000000000000000000, -0.000000000000000000, -1.000000000000000000 ) ) ;
#13636 = DIRECTION ( 'NONE',  ( -0.1566598588826321192, 0.9876526153536342445, 7.798540720466730171E-17 ) ) ;
#13637 = CARTESIAN_POINT ( 'NONE',  ( -16.70711637639958269, -17.83733276090463704, 21.65063509461101532 ) ) ;
#13638 = DIRECTION ( 'NONE',  ( -0.1615579233078773547, 0.9868632313631134911, 0.000000000000000000 ) ) ;
#13639 = AXIS2_PLACEMENT_3D ( 'NONE', #17049, #9819, #2610 ) ;
#13640 = FACE_OUTER_BOUND ( 'NONE', #6395, .T. ) ;
#13641 = AXIS2_PLACEMENT_3D ( 'NONE', #9172, #9072, #170 ) ;
#13642 = CYLINDRICAL_SURFACE ( 'NONE', #3001, 3.000000000000000000 ) ;
#13643 = ORIENTED_EDGE ( 'NONE', *, *, #17194, .F. ) ;
#13644 = ORIENTED_EDGE ( 'NONE', *, *, #14501, .T. ) ;
#13645 = ORIENTED_EDGE ( 'NONE', *, *, #17369, .F. ) ;
#13646 = CARTESIAN_POINT ( 'NONE',  ( -81.73462711737164454, 33.01666666666666572, 35.00000000000000000 ) ) ;
#13647 = EDGE_CURVE ( 'NONE', #9148, #16586, #12250, .T. ) ;
#13648 = VECTOR ( 'NONE', #11380, 1000.000000000000000 ) ;
#13649 = ADVANCED_FACE ( 'NONE', ( #8491, #2514 ), #3809, .F. ) ;
#13650 = FACE_BOUND ( 'NONE', #7580, .T. ) ;
#13651 = EDGE_CURVE ( 'NONE', #8612, #9635, #3158, .T. ) ;
#13652 = FACE_OUTER_BOUND ( 'NONE', #6182, .T. ) ;
#13653 = CIRCLE ( 'NONE', #2170, 1.500000000000001332 ) ;
#13654 = APPLICATION_CONTEXT ( 'automotive_design' ) ;
#13655 = CARTESIAN_POINT ( 'NONE',  ( -36.46016868347218320, -20.97052993855728076, 21.65063509461102242 ) ) ;
#13656 = VERTEX_POINT ( 'NONE', #17039 ) ;
#13657 = AXIS2_PLACEMENT_3D ( 'NONE', #7867, #3674, #15245 ) ;
#13658 = CARTESIAN_POINT ( 'NONE',  ( -55.39028668595378946, -86.74117162932616054, -8.660254037844385522 ) ) ;
#13659 = DIRECTION ( 'NONE',  ( -0.1566598588826321192, 0.9876526153536342445, 7.798540720466730171E-17 ) ) ;
#13660 = CARTESIAN_POINT ( 'NONE',  ( 2.841582609732560272, -19.79905851890276836, 1.367155779166322214E-14 ) ) ;
#13661 = VECTOR ( 'NONE', #12900, 1000.000000000000000 ) ;
#13662 = CARTESIAN_POINT ( 'NONE',  ( -51.27495791377664602, -23.32042782179674134, -12.99038105676658006 ) ) ;
#13663 = ORIENTED_EDGE ( 'NONE', *, *, #5464, .F. ) ;
#13664 = ORIENTED_EDGE ( 'NONE', *, *, #6028, .T. ) ;
#13665 = LINE ( 'NONE', #13952, #6344 ) ;
#13666 = EDGE_CURVE ( 'NONE', #13460, #7022, #15279, .T. ) ;
#13667 = CARTESIAN_POINT ( 'NONE',  ( -29.05277406831996245, -19.79558099693753803, 8.660254037844417496 ) ) ;
#13668 = AXIS2_PLACEMENT_3D ( 'NONE', #6378, #17955, #4920 ) ;
#13669 = ORIENTED_EDGE ( 'NONE', *, *, #11636, .F. ) ;
#13670 = EDGE_CURVE ( 'NONE', #8498, #44, #13750, .T. ) ;
#13671 = DIRECTION ( 'NONE',  ( -0.1566598588826321747, 0.9876526153536343555, 0.000000000000000000 ) ) ;
#13672 = CARTESIAN_POINT ( 'NONE',  ( -170.1307959478061491, 32.02908766448062750, 4.051035741711875637 ) ) ;
#13673 = CARTESIAN_POINT ( 'NONE',  ( -172.8790805967747133, 56.46496941305928630, -2.601363783521513540 ) ) ;
#13674 = ORIENTED_EDGE ( 'NONE', *, *, #16114, .F. ) ;
#13675 = AXIS2_PLACEMENT_3D ( 'NONE', #3457, #17820, #9256 ) ;
#13676 = DIRECTION ( 'NONE',  ( 0.000000000000000000, 0.000000000000000000, 1.000000000000000000 ) ) ;
#13677 = DIRECTION ( 'NONE',  ( -0.000000000000000000, -0.000000000000000000, -1.000000000000000000 ) ) ;
#13678 = DIRECTION ( 'NONE',  ( -0.1566598588826321747, 0.9876526153536343555, 0.000000000000000000 ) ) ;
#13679 = FACE_OUTER_BOUND ( 'NONE', #13836, .T. ) ;
#13680 = DIRECTION ( 'NONE',  ( 0.000000000000000000, 0.000000000000000000, 1.000000000000000000 ) ) ;
#13681 = CARTESIAN_POINT ( 'NONE',  ( -18.39294862037050393, -23.16724548487935564, -17.32050807568878170 ) ) ;
#13682 = DIRECTION ( 'NONE',  ( -0.1566598588826321192, 0.9876526153536342445, 7.798540720466730171E-17 ) ) ;
#13683 = ORIENTED_EDGE ( 'NONE', *, *, #12572, .F. ) ;
#13684 = EDGE_LOOP ( 'NONE', ( #4017, #10789, #9329, #4325 ) ) ;
#13685 = AXIS2_PLACEMENT_3D ( 'NONE', #602, #15185, #17773 ) ;
#13686 = FACE_OUTER_BOUND ( 'NONE', #5180, .T. ) ;
#13687 = ORIENTED_EDGE ( 'NONE', *, *, #5076, .F. ) ;
#13688 = ORIENTED_EDGE ( 'NONE', *, *, #7708, .F. ) ;
#13689 = EDGE_LOOP ( 'NONE', ( #13034, #9293 ) ) ;
#13690 = VERTEX_POINT ( 'NONE', #6888 ) ;
#13691 = CARTESIAN_POINT ( 'NONE',  ( -16.70711637639958269, -17.83733276090463704, -4.330127018922180326 ) ) ;
#13692 = ADVANCED_FACE ( 'NONE', ( #15395 ), #1207, .F. ) ;
#13693 = DIRECTION ( 'NONE',  ( -0.1566598588826321192, 0.9876526153536342445, 7.798540720466730171E-17 ) ) ;
#13694 = EDGE_CURVE ( 'NONE', #18004, #15166, #17734, .T. ) ;
#13695 = ORIENTED_EDGE ( 'NONE', *, *, #15526, .F. ) ;
#13696 = FACE_OUTER_BOUND ( 'NONE', #14411, .T. ) ;
#13697 = CYLINDRICAL_SURFACE ( 'NONE', #7640, 1.500000000000001554 ) ;
#13698 = ADVANCED_FACE ( 'NONE', ( #3724 ), #9893, .T. ) ;
#13699 = DIRECTION ( 'NONE',  ( -0.9876526153536341335, -0.1566598588826327021, 0.000000000000000000 ) ) ;
#13700 = CARTESIAN_POINT ( 'NONE',  ( -70.00000000000000000, 44.99999999999999289, -2.500000000000000000 ) ) ;
#13701 = VERTEX_POINT ( 'NONE', #2698 ) ;
#13702 = FACE_OUTER_BOUND ( 'NONE', #640, .T. ) ;
#13703 = ORIENTED_EDGE ( 'NONE', *, *, #5880, .T. ) ;
#13704 = VERTEX_POINT ( 'NONE', #9734 ) ;
#13705 = EDGE_LOOP ( 'NONE', ( #10148, #7716 ) ) ;
#13706 = DIRECTION ( 'NONE',  ( 1.000000000000000000, 0.000000000000000000, 0.000000000000000000 ) ) ;
#13707 = AXIS2_PLACEMENT_3D ( 'NONE', #13713, #2256, #16795 ) ;
#13708 = FACE_OUTER_BOUND ( 'NONE', #9822, .T. ) ;
#13709 = ORIENTED_EDGE ( 'NONE', *, *, #18707, .F. ) ;
#13710 = ORIENTED_EDGE ( 'NONE', *, *, #17153, .F. ) ;
#13711 = CARTESIAN_POINT ( 'NONE',  ( -11.76885329963143079, -17.05403346649147878, 21.65063509461101532 ) ) ;
#13712 = CARTESIAN_POINT ( 'NONE',  ( -18.35331361019266794, -80.86642692122748599, 21.65063509461101532 ) ) ;
#13713 = CARTESIAN_POINT ( 'NONE',  ( -66.08974714408107332, -25.67032570503623035, 21.65063509461102242 ) ) ;
#13714 = DIRECTION ( 'NONE',  ( -0.000000000000000000, -0.000000000000000000, -1.000000000000000000 ) ) ;
#13715 = EDGE_CURVE ( 'NONE', #4657, #12177, #14392, .T. ) ;
#13716 = DIRECTION ( 'NONE',  ( 0.000000000000000000, 0.000000000000000000, 1.000000000000000000 ) ) ;
#13717 = DIRECTION ( 'NONE',  ( -0.9876526153536336894, -0.1566598588826349503, 0.000000000000000000 ) ) ;
#13718 = CYLINDRICAL_SURFACE ( 'NONE', #1175, 1.500000000000001554 ) ;
#13719 = VERTEX_POINT ( 'NONE', #4007 ) ;
#13720 = DIRECTION ( 'NONE',  ( 0.000000000000000000, 0.000000000000000000, 1.000000000000000000 ) ) ;
#13721 = CARTESIAN_POINT ( 'NONE',  ( -1.109027851681973598, -20.42569795443330349, -21.65063509461098334 ) ) ;
#13722 = EDGE_CURVE ( 'NONE', #14919, #12166, #5913, .T. ) ;
#13723 = SHAPE_REPRESENTATION ( 'Ergonomic Handle Grip Sleeves', ( #18772 ), #9301 ) ;
#13724 = VERTEX_POINT ( 'NONE', #18588 ) ;
#13725 = DIRECTION ( 'NONE',  ( 0.000000000000000000, 1.000000000000000000, -0.000000000000000000 ) ) ;
#13726 = ORIENTED_EDGE ( 'NONE', *, *, #5544, .F. ) ;
#13727 = EDGE_LOOP ( 'NONE', ( #7578, #7982 ) ) ;
#13728 = ORIENTED_EDGE ( 'NONE', *, *, #14044, .F. ) ;
#13729 = CARTESIAN_POINT ( 'NONE',  ( -22.34355908178503469, -23.79388492040988012, 12.99038105676661736 ) ) ;
#13730 = ORIENTED_EDGE ( 'NONE', *, *, #9598, .F. ) ;
#13731 = VERTEX_POINT ( 'NONE', #11019 ) ;
#13732 = FACE_BOUND ( 'NONE', #7765, .T. ) ;
#13733 = ORIENTED_EDGE ( 'NONE', *, *, #4273, .F. ) ;
#13734 = SURFACE_SIDE_STYLE ('',( #7978 ) ) ;
#13735 = VECTOR ( 'NONE', #684, 1000.000000000000000 ) ;
#13736 = VERTEX_POINT ( 'NONE', #6704 ) ;
#13737 = EDGE_CURVE ( 'NONE', #14596, #13134, #13164, .T. ) ;
#13738 = EDGE_CURVE ( 'NONE', #5191, #17705, #165, .T. ) ;
#13739 = EDGE_LOOP ( 'NONE', ( #5062, #954, #13469, #8369 ) ) ;
#13740 = CYLINDRICAL_SURFACE ( 'NONE', #1870, 1.500000000000001554 ) ;
#13741 = CARTESIAN_POINT ( 'NONE',  ( 59.44021041145193607, -44.12097743988038445, 19.99999999999998579 ) ) ;
#13742 = EDGE_LOOP ( 'NONE', ( #6090, #14413, #1008, #4635, #16354, #1719, #15097 ) ) ;
#13743 = DIRECTION ( 'NONE',  ( -0.1566598588826321192, 0.9876526153536342445, 7.798540720466731404E-17 ) ) ;
#13745 = EDGE_CURVE ( 'NONE', #4400, #8333, #11930, .T. ) ;
#13744 = DIRECTION ( 'NONE',  ( 0.000000000000000000, 0.000000000000000000, 1.000000000000000000 ) ) ;
#13746 = DIRECTION ( 'NONE',  ( -0.9201637183752250371, 0.3915338189555017667, 2.458192809297184296E-16 ) ) ;
#13747 = ORIENTED_EDGE ( 'NONE', *, *, #128, .T. ) ;
#13748 = EDGE_LOOP ( 'NONE', ( #8922, #3729 ) ) ;
#13749 = DIRECTION ( 'NONE',  ( -0.9876526153536341335, -0.1566598588826327021, 0.000000000000000000 ) ) ;
#13750 = CIRCLE ( 'NONE', #5612, 2.000000000000000000 ) ;
#13751 = FACE_OUTER_BOUND ( 'NONE', #7761, .T. ) ;
#13752 = ORIENTED_EDGE ( 'NONE', *, *, #17993, .F. ) ;
#13753 = ORIENTED_EDGE ( 'NONE', *, *, #13424, .F. ) ;
#13754 = DIRECTION ( 'NONE',  ( -0.000000000000000000, -0.000000000000000000, 1.000000000000000000 ) ) ;
#13755 = ORIENTED_EDGE ( 'NONE', *, *, #17637, .T. ) ;
#13756 = CARTESIAN_POINT ( 'NONE',  ( -128.0119535342734878, -15.18399252164955548, 3.146712427857099481 ) ) ;
#13757 = CARTESIAN_POINT ( 'NONE',  ( -167.6743523352497789, 32.11760736101219038, 2.500000000000000888 ) ) ;
#13758 = CARTESIAN_POINT ( 'NONE',  ( -173.0699421713717925, 56.41947239034702477, -2.662644313562635201 ) ) ;
#13759 = EDGE_CURVE ( 'NONE', #18515, #10629, #921, .T. ) ;
#13760 = CARTESIAN_POINT ( 'NONE',  ( -66.25446545484369665, -88.46443007703511796, -4.330127018922185655 ) ) ;
#13761 = VECTOR ( 'NONE', #15783, 1000.000000000000000 ) ;
#13762 = DIRECTION ( 'NONE',  ( -0.1566598588826321747, 0.9876526153536343555, 0.000000000000000000 ) ) ;
#13763 = APPLICATION_PROTOCOL_DEFINITION ( 'draft international standard', 'automotive_design', 1998, #3244 ) ;
#13764 = EDGE_CURVE ( 'NONE', #6194, #15676, #1689, .T. ) ;
#13765 = EDGE_CURVE ( 'NONE', #14520, #16637, #4693, .T. ) ;
#13766 = EDGE_CURVE ( 'NONE', #697, #6194, #18387, .T. ) ;
#13767 = LINE ( 'NONE', #3805, #14221 ) ;
#13768 = SURFACE_STYLE_USAGE ( .BOTH. , #8004 ) ;
#13770 = ADVANCED_FACE ( 'NONE', ( #4205, #9989, #7359 ), #17223, .F. ) ;
#13769 = CARTESIAN_POINT ( 'NONE',  ( -1.109027851681966492, -20.42569795443330349, 4.330127018922212301 ) ) ;
#13771 = CARTESIAN_POINT ( 'NONE',  ( -71.23236354178969520, -31.54854793510013877, -8.660254037844380193 ) ) ;
#13772 = ORIENTED_EDGE ( 'NONE', *, *, #6220, .T. ) ;
#13773 = EDGE_LOOP ( 'NONE', ( #5638, #10790, #10021, #8920 ) ) ;
#13774 = DIRECTION ( 'NONE',  ( -0.9876526153536341335, -0.1566598588826327021, 0.000000000000000000 ) ) ;
#13775 = AXIS2_PLACEMENT_3D ( 'NONE', #16175, #14836, #14592 ) ;
#13776 = VERTEX_POINT ( 'NONE', #8756 ) ;
#13777 = VECTOR ( 'NONE', #8258, 1000.000000000000000 ) ;
#13778 = EDGE_LOOP ( 'NONE', ( #5995, #18148, #3637, #1720 ) ) ;
#13779 = CYLINDRICAL_SURFACE ( 'NONE', #15341, 1.500000000000001554 ) ;
#13780 = DIRECTION ( 'NONE',  ( -0.9876526153536344665, -0.1566598588826304539, 0.000000000000000000 ) ) ;
#13781 = AXIS2_PLACEMENT_3D ( 'NONE', #1354, #5887, #3973 ) ;
#13782 = LINE ( 'NONE', #12268, #14938 ) ;
#13783 = ORIENTED_EDGE ( 'NONE', *, *, #17071, .F. ) ;
#13784 = LINE ( 'NONE', #15419, #6740 ) ;
#13785 = EDGE_CURVE ( 'NONE', #14796, #13180, #17600, .T. ) ;
#13786 = LINE ( 'NONE', #455, #1199 ) ;
#13787 = AXIS2_PLACEMENT_3D ( 'NONE', #18319, #8024, #18513 ) ;
#13788 = ORIENTED_EDGE ( 'NONE', *, *, #6994, .T. ) ;
#13789 = CARTESIAN_POINT ( 'NONE',  ( -4.526176995241833367, -78.67318889687062722, -8.660254037844385522 ) ) ;
#13790 = DIRECTION ( 'NONE',  ( -0.9876526153536336894, -0.1566598588826349503, 0.000000000000000000 ) ) ;
#13791 = VERTEX_POINT ( 'NONE', #14638 ) ;
#13792 = CARTESIAN_POINT ( 'NONE',  ( -79.62936786100797804, 31.64307958360170048, 35.00001199999999812 ) ) ;
#13793 = DIRECTION ( 'NONE',  ( -0.1566598588826321192, 0.9876526153536342445, 7.798540720466730171E-17 ) ) ;
#13795 = ORIENTED_EDGE ( 'NONE', *, *, #17511, .T. ) ;
#13794 = CARTESIAN_POINT ( 'NONE',  ( -126.1404785418517918, 9.649298036820672664, -2.500000000000000000 ) ) ;
#13796 = EDGE_CURVE ( 'NONE', #5804, #11671, #15289, .T. ) ;
#13797 = DIRECTION ( 'NONE',  ( -0.1566598588826321192, 0.9876526153536342445, 7.798540720466730171E-17 ) ) ;
#13798 = VERTEX_POINT ( 'NONE', #14448 ) ;
#13799 = AXIS2_PLACEMENT_3D ( 'NONE', #10406, #5970, #11719 ) ;
#13800 = EDGE_LOOP ( 'NONE', ( #1559, #12687, #17896, #9424 ) ) ;
#13801 = ORIENTED_EDGE ( 'NONE', *, *, #6633, .T. ) ;
#13802 = AXIS2_PLACEMENT_3D ( 'NONE', #11683, #17625, #11955 ) ;
#13803 = CYLINDRICAL_SURFACE ( 'NONE', #347, 2.000000000000000000 ) ;
#13804 = ORIENTED_EDGE ( 'NONE', *, *, #5088, .T. ) ;
#13805 = EDGE_LOOP ( 'NONE', ( #12026, #3797, #12588, #1352 ) ) ;
#13806 = CARTESIAN_POINT ( 'NONE',  ( 55.85952145814821534, 6.938893903907228378E-15, 24.99999999999998224 ) ) ;
#13807 = FACE_OUTER_BOUND ( 'NONE', #9016, .T. ) ;
#13808 = ORIENTED_EDGE ( 'NONE', *, *, #11491, .F. ) ;
#13809 = DIRECTION ( 'NONE',  ( -0.1566598588826321747, 0.9876526153536343555, 0.000000000000000000 ) ) ;
#13810 = AXIS2_PLACEMENT_3D ( 'NONE', #13229, #8964, #6047 ) ;
#13811 = DIRECTION ( 'NONE',  ( -0.9876526153536341335, -0.1566598588826327021, 0.000000000000000000 ) ) ;
#13812 = CARTESIAN_POINT ( 'NONE',  ( 11.59211860341529565, 6.314490184041233967, 20.00000000000000000 ) ) ;
#13813 = AXIS2_PLACEMENT_3D ( 'NONE', #14655, #7551, #1594 ) ;
#13814 = AXIS2_PLACEMENT_3D ( 'NONE', #12472, #3824, #7837 ) ;
#13815 = CARTESIAN_POINT ( 'NONE',  ( -67.77557938805200877, -31.00023842901093118, -17.32050807568878170 ) ) ;
#13816 = VERTEX_POINT ( 'NONE', #7526 ) ;
#13817 = DIRECTION ( 'NONE',  ( -0.9876526153536341335, -0.1566598588826327021, 0.000000000000000000 ) ) ;
#13818 = ORIENTED_EDGE ( 'NONE', *, *, #16610, .F. ) ;
#13819 = LINE ( 'NONE', #12008, #6438 ) ;
#13820 = CARTESIAN_POINT ( 'NONE',  ( -80.87641299911182102, 2.735640769738576505, 2.577396323571959691 ) ) ;
#13821 = AXIS2_PLACEMENT_3D ( 'NONE', #8489, #2961, #15782 ) ;
#13822 = COLOUR_RGB ( '', 0.72549020, 0.75294118, 0.79215686) ;
#13823 = EDGE_CURVE ( 'NONE', #15970, #5513, #11397, .T. ) ;
#13824 = AXIS2_PLACEMENT_3D ( 'NONE', #18231, #8241, #15434 ) ;
#13825 = ORIENTED_EDGE ( 'NONE', *, *, #15389, .T. ) ;
#13826 = DIRECTION ( 'NONE',  ( 1.000000000000000000, 0.000000000000000000, -2.887450008416415878E-16 ) ) ;
#13827 = EDGE_CURVE ( 'NONE', #13088, #12921, #14094, .T. ) ;
#13828 = ORIENTED_EDGE ( 'NONE', *, *, #1446, .F. ) ;
#13829 = CARTESIAN_POINT ( 'NONE',  ( -10.28737437660097775, -16.81904367816753165, 12.99038105676661381 ) ) ;
#13830 = ORIENTED_EDGE ( 'NONE', *, *, #13168, .T. ) ;
#13831 = ORIENTED_EDGE ( 'NONE', *, *, #3146, .F. ) ;
#13832 = ORIENTED_EDGE ( 'NONE', *, *, #7142, .F. ) ;
#13833 = FACE_OUTER_BOUND ( 'NONE', #4511, .T. ) ;
#13834 = VECTOR ( 'NONE', #9838, 1000.000000000000000 ) ;
#13835 = EDGE_CURVE ( 'NONE', #6362, #6405, #4093, .T. ) ;
#13836 = EDGE_LOOP ( 'NONE', ( #6783, #14977, #923, #15432 ) ) ;
#13837 = FACE_BOUND ( 'NONE', #16344, .T. ) ;
#13838 = LINE ( 'NONE', #2567, #6754 ) ;
#13839 = FACE_OUTER_BOUND ( 'NONE', #3051, .T. ) ;
#13840 = DIRECTION ( 'NONE',  ( -0.1566598588826321192, 0.9876526153536342445, 7.798540720466731404E-17 ) ) ;
#13841 = ORIENTED_EDGE ( 'NONE', *, *, #11766, .F. ) ;
#13842 = LINE ( 'NONE', #9590, #16045 ) ;
#13843 = DIRECTION ( 'NONE',  ( -0.1566598588826321192, 0.9876526153536342445, 7.798540720466730171E-17 ) ) ;
#13844 = AXIS2_PLACEMENT_3D ( 'NONE', #14651, #13211, #7102 ) ;
#13845 = VERTEX_POINT ( 'NONE', #8588 ) ;
#13846 = ORIENTED_EDGE ( 'NONE', *, *, #1522, .F. ) ;
#13847 = DIRECTION ( 'NONE',  ( -0.1566598588826321747, 0.9876526153536343555, 0.000000000000000000 ) ) ;
#13848 = CIRCLE ( 'NONE', #5993, 1.500000000000001332 ) ;
#13849 = CARTESIAN_POINT ( 'NONE',  ( -169.0061012838959584, 31.93472873824967806, -2.921574671186277339 ) ) ;
#13850 = ORIENTED_EDGE ( 'NONE', *, *, #669, .T. ) ;
#13851 = ORIENTED_EDGE ( 'NONE', *, *, #6196, .T. ) ;
#13852 = CARTESIAN_POINT ( 'NONE',  ( -84.23462711737164454, 33.01666666666666572, -35.00000000000000000 ) ) ;
#13853 = EDGE_CURVE ( 'NONE', #482, #15938, #13107, .T. ) ;
#13854 = ORIENTED_EDGE ( 'NONE', *, *, #7682, .T. ) ;
#13855 = ORIENTED_EDGE ( 'NONE', *, *, #9686, .T. ) ;
#13856 = DIRECTION ( 'NONE',  ( -1.000000000000000000, 0.000000000000000000, 0.000000000000000000 ) ) ;
#13857 = CARTESIAN_POINT ( 'NONE',  ( -168.2608473273504615, 32.01710443037316622, 2.601363783521516648 ) ) ;
#13858 = CIRCLE ( 'NONE', #1485, 29.12282187559191016 ) ;
#13859 = EDGE_CURVE ( 'NONE', #1906, #4836, #13192, .T. ) ;
#13860 = DIRECTION ( 'NONE',  ( -0.1566598588826321192, 0.9876526153536342445, 7.798540720466730171E-17 ) ) ;
#13861 = AXIS2_PLACEMENT_3D ( 'NONE', #16701, #17844, #866 ) ;
#13862 = CIRCLE ( 'NONE', #12337, 1.500000000000000888 ) ;
#13863 = CARTESIAN_POINT ( 'NONE',  ( -31.52190560670403841, -20.18723064414411184, -4.330127018922180326 ) ) ;
#13864 =( LENGTH_UNIT ( ) NAMED_UNIT ( * ) SI_UNIT ( .MILLI., .METRE. ) );
#13865 = CIRCLE ( 'NONE', #13254, 1.500000000000000444 ) ;
#13866 = CARTESIAN_POINT ( 'NONE',  ( -129.1404785418517918, -2.850701963179328668, 9.951701414186818625E-16 ) ) ;
#13867 = CARTESIAN_POINT ( 'NONE',  ( -79.20163718375225415, 48.91533818955501545, 2.500000000000000000 ) ) ;
#13868 = CIRCLE ( 'NONE', #5732, 1.500000000000000888 ) ;
#13869 = DIRECTION ( 'NONE',  ( -0.000000000000000000, -0.000000000000000000, -1.000000000000000000 ) ) ;
#13870 = CARTESIAN_POINT ( 'NONE',  ( -74.19532138785061193, -32.01852751174804013, -8.660254037844380193 ) ) ;
#13871 = ORIENTED_EDGE ( 'NONE', *, *, #11793, .F. ) ;
#13872 = ORIENTED_EDGE ( 'NONE', *, *, #6910, .T. ) ;
#13873 = PLANE ( 'NONE',  #15727 ) ;
#13874 = FACE_OUTER_BOUND ( 'NONE', #10840, .T. ) ;
#13875 = EDGE_CURVE ( 'NONE', #15554, #16333, #16514, .T. ) ;
#13876 = AXIS2_PLACEMENT_3D ( 'NONE', #4737, #13447, #4648 ) ;
#13877 = ORIENTED_EDGE ( 'NONE', *, *, #3123, .F. ) ;
#13878 = VECTOR ( 'NONE', #10033, 1000.000000000000000 ) ;
#13879 = AXIS2_PLACEMENT_3D ( 'NONE', #3562, #848, #6626 ) ;
#13880 = ORIENTED_EDGE ( 'NONE', *, *, #17707, .T. ) ;
#13881 = ORIENTED_EDGE ( 'NONE', *, *, #2209, .F. ) ;
#13882 = VERTEX_POINT ( 'NONE', #15961 ) ;
#13883 = CARTESIAN_POINT ( 'NONE',  ( -74.97862068226375243, -27.08026443497990599, 1.908195823574487804E-14 ) ) ;
#13884 = CARTESIAN_POINT ( 'NONE',  ( -56.91140061916208026, -29.27697998130198442, 12.99038105676661736 ) ) ;
#13885 = ADVANCED_FACE ( 'NONE', ( #1386 ), #7168, .F. ) ;
#13886 = ADVANCED_FACE ( 'NONE', ( #12913, #4487, #225 ), #10164, .T. ) ;
#13887 = DIRECTION ( 'NONE',  ( -0.1566598588826321747, 0.9876526153536343555, 0.000000000000000000 ) ) ;
#13888 = EDGE_CURVE ( 'NONE', #2138, #11597, #16553, .T. ) ;
#13889 = DIRECTION ( 'NONE',  ( -0.1566598588826321192, 0.9876526153536342445, 7.798540720466730171E-17 ) ) ;
#13890 = DIRECTION ( 'NONE',  ( 0.1856185419698762884, -0.9826218788918641422, 0.000000000000000000 ) ) ;
#13891 = VECTOR ( 'NONE', #9395, 1000.000000000000000 ) ;
#13892 = ORIENTED_EDGE ( 'NONE', *, *, #5305, .T. ) ;
#13893 = CARTESIAN_POINT ( 'NONE',  ( -8.516422466834198346, -21.60064689605303911, 8.660254037844413944 ) ) ;
#13894 = VECTOR ( 'NONE', #2890, 1000.000000000000114 ) ;
#13895 = CIRCLE ( 'NONE', #12944, 1.500000000000001332 ) ;
#13896 = FACE_OUTER_BOUND ( 'NONE', #2142, .T. ) ;
#13897 = AXIS2_PLACEMENT_3D ( 'NONE', #726, #13238, #14767 ) ;
#13898 = VECTOR ( 'NONE', #6501, 1000.000000000000000 ) ;
#13899 = DIRECTION ( 'NONE',  ( -0.1566598588826321192, 0.9876526153536342445, 7.798540720466730171E-17 ) ) ;
#13900 = ORIENTED_EDGE ( 'NONE', *, *, #14368, .T. ) ;
#13901 = DIRECTION ( 'NONE',  ( -0.1566598588826321192, 0.9876526153536342445, 7.798540720466730171E-17 ) ) ;
#13902 = CARTESIAN_POINT ( 'NONE',  ( -4.361458684479201153, -15.87908452487173427, -17.32050807568878170 ) ) ;
#13903 = EDGE_LOOP ( 'NONE', ( #18552, #9365 ) ) ;
#13904 = AXIS2_PLACEMENT_3D ( 'NONE', #15239, #5300, #6455 ) ;
#13905 = VERTEX_POINT ( 'NONE', #4665 ) ;
#13906 = AXIS2_PLACEMENT_3D ( 'NONE', #16956, #12550, #1219 ) ;
#13907 = LINE ( 'NONE', #667, #13215 ) ;
#13908 = EDGE_LOOP ( 'NONE', ( #6780, #14390 ) ) ;
#13909 = ORIENTED_EDGE ( 'NONE', *, *, #3653, .T. ) ;
#13910 = CIRCLE ( 'NONE', #6670, 1.499999999999999556 ) ;
#13911 = ADVANCED_FACE ( 'NONE', ( #2204 ), #12137, .F. ) ;
#13912 = VECTOR ( 'NONE', #13359, 1000.000000000000000 ) ;
#13913 = CARTESIAN_POINT ( 'NONE',  ( -34.68921677370540380, -25.75213315644277046, -8.660254037844380193 ) ) ;
#13914 = CYLINDRICAL_SURFACE ( 'NONE', #17701, 1.500000000000001554 ) ;
#13915 = DIRECTION ( 'NONE',  ( 0.000000000000000000, 0.000000000000000000, 1.000000000000000000 ) ) ;
#13916 = DIRECTION ( 'NONE',  ( -0.1566598588826321192, 0.9876526153536342445, 7.798540720466731404E-17 ) ) ;
#13917 = EDGE_CURVE ( 'NONE', #9536, #491, #16239, .T. ) ;
#13918 = CIRCLE ( 'NONE', #1250, 1.499999999999999556 ) ;
#13919 = DIRECTION ( 'NONE',  ( 8.693966348389027220E-17, -1.991237296706374949E-16, 1.000000000000000000 ) ) ;
#13920 = DIRECTION ( 'NONE',  ( -0.9876526153536336894, -0.1566598588826349503, 0.000000000000000000 ) ) ;
#13921 = AXIS2_PLACEMENT_3D ( 'NONE', #14423, #8564, #5427 ) ;
#13922 = CARTESIAN_POINT ( 'NONE',  ( -47.81817376003892406, -22.77211831570753731, 4.330127018922218518 ) ) ;
#13923 = LINE ( 'NONE', #973, #13777 ) ;
#13924 = ORIENTED_EDGE ( 'NONE', *, *, #16765, .T. ) ;
#13925 = AXIS2_PLACEMENT_3D ( 'NONE', #13741, #3782, #5425 ) ;
#13926 = CARTESIAN_POINT ( 'NONE',  ( -73.49714175923330117, -26.84527464665596597, 17.32050807568882078 ) ) ;
#13927 = CIRCLE ( 'NONE', #6690, 1.500000000000000888 ) ;
#13928 = CARTESIAN_POINT ( 'NONE',  ( -6.830590222863280658, -16.27073417207831696, 21.65063509461101532 ) ) ;
#13929 = ORIENTED_EDGE ( 'NONE', *, *, #1377, .T. ) ;
#13930 = ORIENTED_EDGE ( 'NONE', *, *, #17640, .T. ) ;
#13931 = CIRCLE ( 'NONE', #10901, 1.500000000000001332 ) ;
#13932 = VERTEX_POINT ( 'NONE', #16442 ) ;
#13933 = DIRECTION ( 'NONE',  ( -0.9876526153536336894, -0.1566598588826349503, 0.000000000000000000 ) ) ;
#13934 = AXIS2_PLACEMENT_3D ( 'NONE', #4509, #10292, #8882 ) ;
#13935 = ORIENTED_EDGE ( 'NONE', *, *, #2761, .T. ) ;
#13936 = FACE_BOUND ( 'NONE', #10899, .T. ) ;
#13937 = CARTESIAN_POINT ( 'NONE',  ( -61.35583738825340561, -29.98194934627382224, -17.32050807568878170 ) ) ;
#13938 = EDGE_CURVE ( 'NONE', #16948, #15907, #11933, .T. ) ;
#13939 = AXIS2_PLACEMENT_3D ( 'NONE', #7178, #17420, #17234 ) ;
#13940 = EDGE_CURVE ( 'NONE', #9536, #16948, #1395, .T. ) ;
#13941 = FACE_OUTER_BOUND ( 'NONE', #10201, .T. ) ;
#13942 = AXIS2_PLACEMENT_3D ( 'NONE', #8091, #15493, #5547 ) ;
#13943 = DIRECTION ( 'NONE',  ( -0.1566598588826321192, 0.9876526153536342445, 7.798540720466731404E-17 ) ) ;
#13944 = ADVANCED_FACE ( 'NONE', ( #17976 ), #3509, .F. ) ;
#13945 = DIRECTION ( 'NONE',  ( -1.000000000000000000, -0.000000000000000000, -0.000000000000000000 ) ) ;
#13946 = EDGE_LOOP ( 'NONE', ( #7227, #14011, #12282, #18725 ) ) ;
#13948 = DIRECTION ( 'NONE',  ( 0.000000000000000000, 0.000000000000000000, 1.000000000000000000 ) ) ;
#13947 = AXIS2_PLACEMENT_3D ( 'NONE', #15503, #15399, #16657 ) ;
#13949 = CARTESIAN_POINT ( 'NONE',  ( -17.85948730251583783, -80.78809699178616199, 1.443110928631665584E-14 ) ) ;
#13950 = DIRECTION ( 'NONE',  ( -0.1566598588826321192, 0.9876526153536342445, 7.798540720466731404E-17 ) ) ;
#13951 = VERTEX_POINT ( 'NONE', #7900 ) ;
#13952 = CARTESIAN_POINT ( 'NONE',  ( -67.73594437787414790, -88.69941986535906153, 12.99038105676661203 ) ) ;
#13953 = AXIS2_PLACEMENT_3D ( 'NONE', #7072, #18659, #4189 ) ;
#13954 = DIRECTION ( 'NONE',  ( -0.1566598588826321747, 0.9876526153536343555, 0.000000000000000000 ) ) ;
#13955 = ORIENTED_EDGE ( 'NONE', *, *, #18523, .T. ) ;
#13956 = CARTESIAN_POINT ( 'NONE',  ( -170.4545578613200121, 32.23085387660965750, -4.766626691765356583 ) ) ;
#13957 = ORIENTED_EDGE ( 'NONE', *, *, #10860, .T. ) ;
#13958 = ORIENTED_EDGE ( 'NONE', *, *, #11227, .F. ) ;
#13959 = FACE_OUTER_BOUND ( 'NONE', #8839, .T. ) ;
#13960 = ORIENTED_EDGE ( 'NONE', *, *, #17656, .F. ) ;
#13961 = ORIENTED_EDGE ( 'NONE', *, *, #353, .F. ) ;
#13962 = CARTESIAN_POINT ( 'NONE',  ( -126.9394941819792280, -15.29082033824380638, 2.601363783521511763 ) ) ;
#13963 = AXIS2_PLACEMENT_3D ( 'NONE', #16883, #9665, #6540 ) ;
#13964 = CARTESIAN_POINT ( 'NONE',  ( -168.4551535821700838, 31.98984275266787591, 2.662644313562632536 ) ) ;
#13965 = LINE ( 'NONE', #6980, #8211 ) ;
#13966 = AXIS2_PLACEMENT_3D ( 'NONE', #16887, #3855, #17442 ) ;
#13967 = CARTESIAN_POINT ( 'NONE',  ( -47.48906576312472794, -85.48789275826510448, 8.660254037844412167 ) ) ;
#13968 = LINE ( 'NONE', #8376, #865 ) ;
#13969 = CARTESIAN_POINT ( 'NONE',  ( -49.59961335071795219, 37.20051552679455398, -5.000000000000000888 ) ) ;
#13970 = EDGE_LOOP ( 'NONE', ( #1154, #17178, #4713, #14144 ) ) ;
#13971 = EDGE_CURVE ( 'NONE', #2873, #1264, #13467, .T. ) ;
#13972 = PLANE ( 'NONE',  #8171 ) ;
#13973 = DIRECTION ( 'NONE',  ( -0.1566598588826321192, 0.9876526153536342445, 7.798540720466730171E-17 ) ) ;
#13974 = VERTEX_POINT ( 'NONE', #5024 ) ;
#13975 = DIRECTION ( 'NONE',  ( -0.1566598588826321747, 0.9876526153536343555, 0.000000000000000000 ) ) ;
#13976 = AXIS2_PLACEMENT_3D ( 'NONE', #17877, #10354, #417 ) ;
#13977 = DIRECTION ( 'NONE',  ( 0.000000000000000000, 0.000000000000000000, 1.000000000000000000 ) ) ;
#13978 = ORIENTED_EDGE ( 'NONE', *, *, #7059, .T. ) ;
#13979 = ORIENTED_EDGE ( 'NONE', *, *, #9840, .F. ) ;
#13980 = DIRECTION ( 'NONE',  ( -0.9876526153536341335, -0.1566598588826327021, 0.000000000000000000 ) ) ;
#13981 = ORIENTED_EDGE ( 'NONE', *, *, #1850, .F. ) ;
#13982 = EDGE_CURVE ( 'NONE', #5011, #9895, #12242, .T. ) ;
#13983 = VECTOR ( 'NONE', #11134, 1000.000000000000000 ) ;
#13984 = ORIENTED_EDGE ( 'NONE', *, *, #13647, .T. ) ;
#13985 = ADVANCED_FACE ( 'NONE', ( #10717 ), #16517, .F. ) ;
#13986 = EDGE_LOOP ( 'NONE', ( #9554, #17606, #16189, #12544 ) ) ;
#13987 = ORIENTED_EDGE ( 'NONE', *, *, #16437, .F. ) ;
#13988 = DIRECTION ( 'NONE',  ( -0.9876526153536341335, -0.1566598588826327021, 0.000000000000000000 ) ) ;
#13989 = CARTESIAN_POINT ( 'NONE',  ( -81.73462711737164454, 33.01666666666666572, 30.00000000000002842 ) ) ;
#13990 = AXIS2_PLACEMENT_3D ( 'NONE', #12502, #11068, #16893 ) ;
#13991 = CARTESIAN_POINT ( 'NONE',  ( 3.231158466157551423, 19.73726462726227737, -30.00000000000000000 ) ) ;
#13992 = DIRECTION ( 'NONE',  ( -0.1566598588826321747, 0.9876526153536343555, 0.000000000000000000 ) ) ;
#13993 = CARTESIAN_POINT ( 'NONE',  ( -47.03487446562579066, -27.71038139247566079, -12.99038105676658006 ) ) ;
#13994 = ADVANCED_FACE ( 'NONE', ( #6207 ), #9308, .F. ) ;
#13995 = DIRECTION ( 'NONE',  ( -0.1566598588826321192, 0.9876526153536342445, 7.798540720466730171E-17 ) ) ;
#13996 = SURFACE_SIDE_STYLE ('',( #11238 ) ) ;
#13997 = EDGE_CURVE ( 'NONE', #11883, #4233, #4855, .T. ) ;
#13998 = CARTESIAN_POINT ( 'NONE',  ( -36.66452200441265319, -26.06545287420802737, 17.32050807568881723 ) ) ;
#13999 = VERTEX_POINT ( 'NONE', #15001 ) ;
#14000 = LINE ( 'NONE', #3939, #502 ) ;
#14001 = DIRECTION ( 'NONE',  ( 0.000000000000000000, 1.000000000000000000, 0.000000000000000000 ) ) ;
#14002 = ORIENTED_EDGE ( 'NONE', *, *, #8796, .T. ) ;
#14003 = CARTESIAN_POINT ( 'NONE',  ( -84.16561914167408531, 33.59999999999999432, 30.00000000000000000 ) ) ;
#14004 = EDGE_CURVE ( 'NONE', #2756, #10533, #12227, .T. ) ;
#14005 = CARTESIAN_POINT ( 'NONE',  ( -45.01993422474065198, -85.09624311105852712, 12.99038105676661203 ) ) ;
#14006 = VERTEX_POINT ( 'NONE', #7803 ) ;
#14007 = EDGE_CURVE ( 'NONE', #5362, #3259, #16210, .T. ) ;
#14008 = LINE ( 'NONE', #60, #10499 ) ;
#14009 = DIRECTION ( 'NONE',  ( -0.9876526153536336894, -0.1566598588826350336, 0.000000000000000000 ) ) ;
#14010 = DIRECTION ( 'NONE',  ( -0.1566598588826321192, 0.9876526153536342445, 7.798540720466730171E-17 ) ) ;
#14011 = ORIENTED_EDGE ( 'NONE', *, *, #18162, .T. ) ;
#14012 = ORIENTED_EDGE ( 'NONE', *, *, #4930, .F. ) ;
#14013 = AXIS2_PLACEMENT_3D ( 'NONE', #17461, #4365, #7137 ) ;
#14014 = LINE ( 'NONE', #758, #16730 ) ;
#14015 = DIRECTION ( 'NONE',  ( 0.000000000000000000, 0.000000000000000000, 1.000000000000000000 ) ) ;
#14016 = DIRECTION ( 'NONE',  ( -0.1566598588826321747, 0.9876526153536343555, 0.000000000000000000 ) ) ;
#14017 = DIRECTION ( 'NONE',  ( -0.9876526153536341335, -0.1566598588826327021, 0.000000000000000000 ) ) ;
#14018 = DIRECTION ( 'NONE',  ( -1.000000000000000000, 0.000000000000000000, 0.000000000000000000 ) ) ;
#14019 = DIRECTION ( 'NONE',  ( -0.1566598588826321747, 0.9876526153536343555, 0.000000000000000000 ) ) ;
#14020 = CARTESIAN_POINT ( 'NONE',  ( -39.09401853261887538, -84.15628395776273862, 17.32050807568881368 ) ) ;
#14021 = CARTESIAN_POINT ( 'NONE',  ( -36.62488699423481364, -83.76463431055616127, -12.99038105676658539 ) ) ;
#14022 = ADVANCED_FACE ( 'NONE', ( #17884 ), #14815, .F. ) ;
#14023 = ADVANCED_FACE ( 'NONE', ( #13385 ), #4762, .F. ) ;
#14024 = CARTESIAN_POINT ( 'NONE',  ( -26.74836084069850983, -82.19803572172985184, 12.99038105676661203 ) ) ;
#14025 = CARTESIAN_POINT ( 'NONE',  ( 55.85952145814821534, 6.938893903907228378E-15, -30.00000000000000000 ) ) ;
#14026 = AXIS2_PLACEMENT_3D ( 'NONE', #8967, #451, #13502 ) ;
#14027 = EDGE_CURVE ( 'NONE', #18222, #10290, #7446, .T. ) ;
#14028 = CYLINDRICAL_SURFACE ( 'NONE', #1510, 1.500000000000001554 ) ;
#14029 = ORIENTED_EDGE ( 'NONE', *, *, #16792, .F. ) ;
#14030 = ORIENTED_EDGE ( 'NONE', *, *, #7308, .T. ) ;
#14031 = CYLINDRICAL_SURFACE ( 'NONE', #5346, 139.0000000000000000 ) ;
#14032 = FACE_BOUND ( 'NONE', #8551, .T. ) ;
#14033 = FACE_OUTER_BOUND ( 'NONE', #7457, .T. ) ;
#14034 = EDGE_CURVE ( 'NONE', #9121, #7348, #1101, .T. ) ;
#14035 = DIRECTION ( 'NONE',  ( -0.1566598588826321192, 0.9876526153536342445, 7.798540720466730171E-17 ) ) ;
#14036 = DIRECTION ( 'NONE',  ( -1.000000000000000000, 0.000000000000000000, 0.000000000000000000 ) ) ;
#14037 = DIRECTION ( 'NONE',  ( -0.1566598588826321747, 0.9876526153536343555, 0.000000000000000000 ) ) ;
#14038 = DIRECTION ( 'NONE',  ( -0.9876526153536336894, -0.1566598588826349503, 0.000000000000000000 ) ) ;
#14039 = CYLINDRICAL_SURFACE ( 'NONE', #13921, 1.500000000000001554 ) ;
#14040 = CARTESIAN_POINT ( 'NONE',  ( -14.23798483801550674, -17.44568311369805969, 8.660254037844413944 ) ) ;
#14041 = CARTESIAN_POINT ( 'NONE',  ( -44.03228160938704860, -84.93958325217589334, -17.32050807568878525 ) ) ;
#14042 = CYLINDRICAL_SURFACE ( 'NONE', #3554, 1.500000000000000666 ) ;
#14043 = DIRECTION ( 'NONE',  ( -0.1566598588826321192, 0.9876526153536342445, 7.798540720466731404E-17 ) ) ;
#14044 = EDGE_CURVE ( 'NONE', #17286, #17191, #12431, .T. ) ;
#14045 = DIRECTION ( 'NONE',  ( -0.000000000000000000, -0.000000000000000000, -1.000000000000000000 ) ) ;
#14046 = ORIENTED_EDGE ( 'NONE', *, *, #8292, .T. ) ;
#14047 = ORIENTED_EDGE ( 'NONE', *, *, #13132, .T. ) ;
#14048 = CARTESIAN_POINT ( 'NONE',  ( -14.40270314877813895, -80.23978748569695085, -8.660254037844385522 ) ) ;
#14049 = EDGE_CURVE ( 'NONE', #16555, #5480, #17748, .T. ) ;
#14050 = EDGE_LOOP ( 'NONE', ( #17681, #2427 ) ) ;
#14051 = VERTEX_POINT ( 'NONE', #15475 ) ;
#14052 = CYLINDRICAL_SURFACE ( 'NONE', #2472, 145.0000000000000000 ) ;
#14053 = CARTESIAN_POINT ( 'NONE',  ( -169.0003623166909676, 31.93509481583945586, 2.918139657044721336 ) ) ;
#14054 = ORIENTED_EDGE ( 'NONE', *, *, #9593, .T. ) ;
#14055 = CARTESIAN_POINT ( 'NONE',  ( -2.057045456857760524, -78.28153924966404986, -21.65063509461098690 ) ) ;
#14056 = CARTESIAN_POINT ( 'NONE',  ( -55.39028668595378946, -86.74117162932614633, -17.32050807568878525 ) ) ;
#14057 = CARTESIAN_POINT ( 'NONE',  ( -70.95370422460223381, 45.40580545587239669, 4.440689772049350559 ) ) ;
#14058 =( NAMED_UNIT ( * ) SI_UNIT ( $, .STERADIAN. ) SOLID_ANGLE_UNIT ( ) );
#14059 = CARTESIAN_POINT ( 'NONE',  ( -126.1404785418517918, -15.29729532696464567, -2.500000000000000000 ) ) ;
#14060 = CIRCLE ( 'NONE', #5907, 1.500000000000000888 ) ;
#14061 = CARTESIAN_POINT ( 'NONE',  ( -67.57122606711153878, -25.90531549336016681, -4.330127018922180326 ) ) ;
#14062 = DIRECTION ( 'NONE',  ( -0.000000000000000000, -0.000000000000000000, -1.000000000000000000 ) ) ;
#14063 = DIRECTION ( 'NONE',  ( -1.000000000000000000, 0.000000000000000000, -3.039628882124824168E-17 ) ) ;
#14064 = ORIENTED_EDGE ( 'NONE', *, *, #7277, .F. ) ;
#14065 = ORIENTED_EDGE ( 'NONE', *, *, #13501, .T. ) ;
#14066 = DIRECTION ( 'NONE',  ( -0.1566598588826321192, 0.9876526153536342445, 7.798540720466730171E-17 ) ) ;
#14067 = DIRECTION ( 'NONE',  ( 0.000000000000000000, 0.000000000000000000, 1.000000000000000000 ) ) ;
#14068 = EDGE_CURVE ( 'NONE', #3602, #13155, #1982, .T. ) ;
#14069 = ORIENTED_EDGE ( 'NONE', *, *, #783, .T. ) ;
#14070 = DIRECTION ( 'NONE',  ( -0.9876526153536336894, -0.1566598588826349503, 0.000000000000000000 ) ) ;
#14071 = ORIENTED_EDGE ( 'NONE', *, *, #17095, .F. ) ;
#14072 = ORIENTED_EDGE ( 'NONE', *, *, #9814, .T. ) ;
#14073 = VERTEX_POINT ( 'NONE', #16821 ) ;
#14074 = LINE ( 'NONE', #4018, #12110 ) ;
#14075 = EDGE_CURVE ( 'NONE', #1785, #2756, #3477, .T. ) ;
#14076 = VECTOR ( 'NONE', #4506, 1000.000000000000000 ) ;
#14077 = CARTESIAN_POINT ( 'NONE',  ( -52.42732883989288695, -86.27119205267825919, -8.660254037844385522 ) ) ;
#14078 = EDGE_LOOP ( 'NONE', ( #11926, #3410, #11001, #3237 ) ) ;
#14079 = ADVANCED_BREP_SHAPE_REPRESENTATION ( '', ( #8708, #18772 ), #4452 ) ;
#14080 = CARTESIAN_POINT ( 'NONE',  ( -52.96079015774756726, -28.65034054577146705, -8.660254037844380193 ) ) ;
#14081 = DIRECTION ( 'NONE',  ( -0.1566598588826321747, 0.9876526153536343555, 0.000000000000000000 ) ) ;
#14082 = FACE_OUTER_BOUND ( 'NONE', #2954, .T. ) ;
#14083 = CARTESIAN_POINT ( 'NONE',  ( -306.0881213225399051, -2.850701963179328668, 15.83618137761393463 ) ) ;
#14084 =( NAMED_UNIT ( * ) PLANE_ANGLE_UNIT ( ) SI_UNIT ( $, .RADIAN. ) );
#14085 = EDGE_CURVE ( 'NONE', #11811, #3590, #5244, .T. ) ;
#14086 = PRODUCT_DEFINITION_SHAPE ( 'NONE', 'NONE',  #11363 ) ;
#14087 = FACE_OUTER_BOUND ( 'NONE', #6580, .T. ) ;
#14088 = ORIENTED_EDGE ( 'NONE', *, *, #878, .F. ) ;
#14089 = CARTESIAN_POINT ( 'NONE',  ( -58.68235252892886678, -24.49537676341647696, -17.32050807568878170 ) ) ;
#14090 = CARTESIAN_POINT ( 'NONE',  ( -6.995308533625909320, -79.06483854407720457, -12.99038105676658539 ) ) ;
#14091 = ORIENTED_EDGE ( 'NONE', *, *, #11233, .T. ) ;
#14092 = ORIENTED_EDGE ( 'NONE', *, *, #5274, .T. ) ;
#14093 = DIRECTION ( 'NONE',  ( 0.000000000000000000, 0.000000000000000000, 1.000000000000000000 ) ) ;
#14094 = CIRCLE ( 'NONE', #18683, 1.499999999999999556 ) ;
#14095 = CARTESIAN_POINT ( 'NONE',  ( -78.67340168335934436, 1.237153554093905594, 3.655650250101004417 ) ) ;
#14096 = VERTEX_POINT ( 'NONE', #6573 ) ;
#14097 = DIRECTION ( 'NONE',  ( -0.1566598588826321192, 0.9876526153536342445, 7.798540720466730171E-17 ) ) ;
#14098 = ORIENTED_EDGE ( 'NONE', *, *, #4343, .T. ) ;
#14099 = VECTOR ( 'NONE', #5619, 1000.000000000000000 ) ;
#14100 = EDGE_CURVE ( 'NONE', #14196, #16138, #13173, .T. ) ;
#14101 = LINE ( 'NONE', #12662, #11815 ) ;
#14102 = DIRECTION ( 'NONE',  ( -0.9723968097209870765, -0.2333333333333371951, 0.000000000000000000 ) ) ;
#14103 = DIRECTION ( 'NONE',  ( -0.1566598588826321192, 0.9876526153536342445, 7.798540720466730171E-17 ) ) ;
#14104 = CARTESIAN_POINT ( 'NONE',  ( -90.00000000000000000, 34.99999999999999289, 30.00000000000002842 ) ) ;
#14105 = CARTESIAN_POINT ( 'NONE',  ( -167.4745151998187680, 32.15905408292206147, -2.500000000000000000 ) ) ;
#14106 = EDGE_CURVE ( 'NONE', #14747, #18388, #2290, .T. ) ;
#14107 = CARTESIAN_POINT ( 'NONE',  ( -47.03487446562579066, -27.71038139247566079, -4.330127018922181215 ) ) ;
#14108 = DIRECTION ( 'NONE',  ( -0.1566598588826321192, 0.9876526153536342445, 7.798540720466730171E-17 ) ) ;
#14109 = FACE_OUTER_BOUND ( 'NONE', #10871, .T. ) ;
#14110 = CARTESIAN_POINT ( 'NONE',  ( 55.85952145814821534, 6.938893903907228378E-15, -35.00000000000000000 ) ) ;
#14111 = CARTESIAN_POINT ( 'NONE',  ( -30.04042668367358360, -19.95224085582016826, -4.330127018922180326 ) ) ;
#14112 = CARTESIAN_POINT ( 'NONE',  ( -349.6046375497077179, 10.42115585936045896, 9.951701414186830458E-16 ) ) ;
#14113 = DIRECTION ( 'NONE',  ( 1.000000000000000000, 0.000000000000000000, 0.000000000000000000 ) ) ;
#14114 = CARTESIAN_POINT ( 'NONE',  ( -13.45468554360235203, -22.38394619046619383, 8.660254037844413944 ) ) ;
#14115 = CIRCLE ( 'NONE', #6877, 1.500000000000001332 ) ;
#14116 = ORIENTED_EDGE ( 'NONE', *, *, #16402, .T. ) ;
#14117 = ORIENTED_EDGE ( 'NONE', *, *, #6302, .F. ) ;
#14118 = FACE_OUTER_BOUND ( 'NONE', #17978, .T. ) ;
#14119 = ORIENTED_EDGE ( 'NONE', *, *, #15384, .T. ) ;
#14120 = CARTESIAN_POINT ( 'NONE',  ( -62.83731631128386397, -30.21693913459777647, 1.869203119972154228E-14 ) ) ;
#14121 = ORIENTED_EDGE ( 'NONE', *, *, #18125, .F. ) ;
#14122 = FACE_BOUND ( 'NONE', #779, .T. ) ;
#14123 = AXIS2_PLACEMENT_3D ( 'NONE', #8518, #18321, #6915 ) ;
#14124 = ADVANCED_FACE ( 'NONE', ( #12521 ), #16917, .F. ) ;
#14125 = DIRECTION ( 'NONE',  ( -0.1566598588826321192, 0.9876526153536342445, 7.798540720466730171E-17 ) ) ;
#14126 = EDGE_CURVE ( 'NONE', #537, #17063, #11347, .T. ) ;
#14127 = VECTOR ( 'NONE', #9190, 1000.000000000000000 ) ;
#14128 = EDGE_CURVE ( 'NONE', #15897, #10670, #16532, .T. ) ;
#14129 = ADVANCED_FACE ( 'NONE', ( #15539 ), #5221, .T. ) ;
#14130 = AXIS2_PLACEMENT_3D ( 'NONE', #3439, #3083, #10464 ) ;
#14131 = EDGE_CURVE ( 'NONE', #11609, #4488, #2896, .T. ) ;
#14132 = CARTESIAN_POINT ( 'NONE',  ( -40.57549745564932664, -84.39127374608669641, 17.32050807568881368 ) ) ;
#14133 = ORIENTED_EDGE ( 'NONE', *, *, #13411, .T. ) ;
#14134 = EDGE_CURVE ( 'NONE', #14620, #9571, #9258, .T. ) ;
#14136 = EDGE_LOOP ( 'NONE', ( #3916, #13371, #15625, #2737 ) ) ;
#14135 = AXIS2_PLACEMENT_3D ( 'NONE', #13154, #8814, #4631 ) ;
#14137 = CYLINDRICAL_SURFACE ( 'NONE', #8357, 1.500000000000000666 ) ;
#14138 = DIRECTION ( 'NONE',  ( -0.1566598588826321192, 0.9876526153536342445, 7.798540720466730171E-17 ) ) ;
#14139 = DIRECTION ( 'NONE',  ( -0.1566598588826321192, 0.9876526153536342445, 7.798540720466730171E-17 ) ) ;
#14140 = CIRCLE ( 'NONE', #12605, 1.499999999999999556 ) ;
#14141 = CARTESIAN_POINT ( 'NONE',  ( -49.50400600400985240, -28.10203103968224880, 8.660254037844417496 ) ) ;
#14142 = AXIS2_PLACEMENT_3D ( 'NONE', #17936, #3466, #13617 ) ;
#14143 = CARTESIAN_POINT ( 'NONE',  ( -3.000000000000000000, 3.673940397442059868E-16, 35.00000000000000000 ) ) ;
#14144 = ORIENTED_EDGE ( 'NONE', *, *, #12142, .F. ) ;
#14145 = ORIENTED_EDGE ( 'NONE', *, *, #18581, .F. ) ;
#14146 = ORIENTED_EDGE ( 'NONE', *, *, #10173, .F. ) ;
#14147 = DIRECTION ( 'NONE',  ( -1.000000000000000000, 0.000000000000000000, 0.000000000000000000 ) ) ;
#14148 = VERTEX_POINT ( 'NONE', #10974 ) ;
#14149 = MECHANICAL_DESIGN_GEOMETRIC_PRESENTATION_REPRESENTATION (  '', ( #9605 ), #14495 ) ;
#14150 = DIRECTION ( 'NONE',  ( -0.1566598588826321192, 0.9876526153536342445, 7.798540720466730171E-17 ) ) ;
#14151 = VECTOR ( 'NONE', #3793, 1000.000000000000000 ) ;
#14152 = FACE_OUTER_BOUND ( 'NONE', #16782, .T. ) ;
#14153 = EDGE_CURVE ( 'NONE', #9188, #15027, #6938, .T. ) ;
#14154 = DIRECTION ( 'NONE',  ( -0.1566598588826321192, 0.9876526153536342445, 7.798540720466730171E-17 ) ) ;
#14155 = CARTESIAN_POINT ( 'NONE',  ( -43.04462899403340970, -84.78292339329327376, -4.330127018922185655 ) ) ;
#14156 = UNCERTAINTY_MEASURE_WITH_UNIT (LENGTH_MEASURE( 1.000000000000000082E-05 ), #12532, 'distance_accuracy_value', 'NONE');
#14157 = CARTESIAN_POINT ( 'NONE',  ( -73.57633726875977231, 46.52174766375585335, 2.626980532068773133 ) ) ;
#14158 = CARTESIAN_POINT ( 'NONE',  ( -84.20693962813486166, 32.64562644091790844, -35.00000000000000000 ) ) ;
#14159 = EDGE_CURVE ( 'NONE', #16087, #5366, #16802, .T. ) ;
#14160 = VERTEX_POINT ( 'NONE', #12403 ) ;
#14161 = CARTESIAN_POINT ( 'NONE',  ( -72.71384246482016067, -31.78353772342409300, -8.660254037844380193 ) ) ;
#14162 = DIRECTION ( 'NONE',  ( -0.1566598588826321747, 0.9876526153536343555, 0.000000000000000000 ) ) ;
#14163 = CIRCLE ( 'NONE', #3254, 1.500000000000000444 ) ;
#14164 = CARTESIAN_POINT ( 'NONE',  ( -2.057045456857756971, -78.28153924966404986, 21.65063509461100821 ) ) ;
#14165 = CARTESIAN_POINT ( 'NONE',  ( -50.49165861936349131, -28.25869089856488614, -21.65063509461098334 ) ) ;
#14166 = ORIENTED_EDGE ( 'NONE', *, *, #15667, .F. ) ;
#14167 = VERTEX_POINT ( 'NONE', #2359 ) ;
#14168 = CARTESIAN_POINT ( 'NONE',  ( -77.40662104346073136, 32.93835651487657401, 30.00000000000002132 ) ) ;
#14169 = DIRECTION ( 'NONE',  ( -0.1566598588826321192, 0.9876526153536342445, 7.798540720466731404E-17 ) ) ;
#14170 = VERTEX_POINT ( 'NONE', #9676 ) ;
#14171 = CIRCLE ( 'NONE', #9008, 1.500000000000000444 ) ;
#14172 = DIRECTION ( 'NONE',  ( -0.1566598588826321747, 0.9876526153536343555, 0.000000000000000000 ) ) ;
#14173 = AXIS2_PLACEMENT_3D ( 'NONE', #5558, #16066, #14363 ) ;
#14174 = ORIENTED_EDGE ( 'NONE', *, *, #12886, .T. ) ;
#14175 = DIRECTION ( 'NONE',  ( -0.1566598588826321192, 0.9876526153536342445, 7.798540720466730171E-17 ) ) ;
#14176 = AXIS2_PLACEMENT_3D ( 'NONE', #2866, #8484, #15660 ) ;
#14177 = AXIS2_PLACEMENT_3D ( 'NONE', #5454, #3909, #15498 ) ;
#14178 = DIRECTION ( 'NONE',  ( -0.1566598588826321192, 0.9876526153536342445, 7.798540720466730171E-17 ) ) ;
#14179 =( GEOMETRIC_REPRESENTATION_CONTEXT ( 3 ) GLOBAL_UNCERTAINTY_ASSIGNED_CONTEXT ( ( #6464 ) ) GLOBAL_UNIT_ASSIGNED_CONTEXT ( ( #8318, #10180, #15595 ) ) REPRESENTATION_CONTEXT ( 'NONE', 'WORKASPACE' ) );
#14180 = VERTEX_POINT ( 'NONE', #11163 ) ;
#14181 = CARTESIAN_POINT ( 'NONE',  ( -88.14047854185180597, 6.938893903907228378E-15, -30.00000000000000000 ) ) ;
#14182 = CYLINDRICAL_SURFACE ( 'NONE', #6789, 2.200000000000000178 ) ;
#14183 = CARTESIAN_POINT ( 'NONE',  ( -2.057045456857760524, -78.28153924966404986, -12.99038105676658539 ) ) ;
#14184 = EDGE_CURVE ( 'NONE', #14768, #1614, #9478, .T. ) ;
#14185 = CYLINDRICAL_SURFACE ( 'NONE', #14805, 1.500000000000001554 ) ;
#14186 = ORIENTED_EDGE ( 'NONE', *, *, #17236, .T. ) ;
#14188 = DIRECTION ( 'NONE',  ( -0.9876526153536341335, -0.1566598588826327021, 0.000000000000000000 ) ) ;
#14187 = AXIS2_PLACEMENT_3D ( 'NONE', #7904, #15196, #3789 ) ;
#14189 = DIRECTION ( 'NONE',  ( -0.1566598588826321192, 0.9876526153536342445, 7.798540720466730171E-17 ) ) ;
#14190 = VECTOR ( 'NONE', #6526, 1000.000000000000000 ) ;
#14191 = DIRECTION ( 'NONE',  ( 0.000000000000000000, 0.000000000000000000, 1.000000000000000000 ) ) ;
#14192 = ORIENTED_EDGE ( 'NONE', *, *, #12697, .F. ) ;
#14193 = CARTESIAN_POINT ( 'NONE',  ( -80.15829819844529425, 31.05859487262427265, 35.00001199999999812 ) ) ;
#14194 = ADVANCED_FACE ( 'NONE', ( #3961 ), #12674, .F. ) ;
#14195 = CIRCLE ( 'NONE', #3869, 1.499999999999999556 ) ;
#14196 = VERTEX_POINT ( 'NONE', #8152 ) ;
#14197 = CARTESIAN_POINT ( 'NONE',  ( -43.08426400421126345, -27.08374195694514341, -8.660254037844380193 ) ) ;
#14198 = EDGE_LOOP ( 'NONE', ( #3412, #5381 ) ) ;
#14199 = ORIENTED_EDGE ( 'NONE', *, *, #18121, .T. ) ;
#14200 = ORIENTED_EDGE ( 'NONE', *, *, #14901, .F. ) ;
#14201 = AXIS2_PLACEMENT_3D ( 'NONE', #7058, #17190, #8731 ) ;
#14202 = CARTESIAN_POINT ( 'NONE',  ( -67.24211807019732134, -88.62108993591775175, 17.32050807568881368 ) ) ;
#14203 = AXIS2_PLACEMENT_3D ( 'NONE', #16082, #1591, #72 ) ;
#14204 = CARTESIAN_POINT ( 'NONE',  ( -15.22563745336913144, -17.60234297258069347, 21.65063509461101177 ) ) ;
#14205 = AXIS2_PLACEMENT_3D ( 'NONE', #10732, #4951, #14736 ) ;
#14206 = DIRECTION ( 'NONE',  ( 0.000000000000000000, 0.000000000000000000, 1.000000000000000000 ) ) ;
#14207 = CYLINDRICAL_SURFACE ( 'NONE', #15490, 1.500000000000001554 ) ;
#14208 = FACE_OUTER_BOUND ( 'NONE', #8429, .T. ) ;
#14209 = FACE_OUTER_BOUND ( 'NONE', #15003, .T. ) ;
#14210 = FACE_OUTER_BOUND ( 'NONE', #9043, .T. ) ;
#14211 = CARTESIAN_POINT ( 'NONE',  ( -4.526176995241833367, -78.67318889687062722, 8.660254037844408614 ) ) ;
#14212 = ORIENTED_EDGE ( 'NONE', *, *, #14791, .T. ) ;
#14213 = LINE ( 'NONE', #4050, #11656 ) ;
#14214 = AXIS2_PLACEMENT_3D ( 'NONE', #18750, #4298, #3999 ) ;
#14215 = AXIS2_PLACEMENT_3D ( 'NONE', #647, #9538, #2327 ) ;
#14216 = DIRECTION ( 'NONE',  ( -0.9876526153536341335, -0.1566598588826327021, 0.000000000000000000 ) ) ;
#14217 = DIRECTION ( 'NONE',  ( -0.1566598588826321747, 0.9876526153536343555, 0.000000000000000000 ) ) ;
#14218 = EDGE_CURVE ( 'NONE', #17604, #3060, #13923, .T. ) ;
#14219 = CIRCLE ( 'NONE', #13601, 1.500000000000000888 ) ;
#14220 = EDGE_LOOP ( 'NONE', ( #8267, #3209, #3644, #11867 ) ) ;
#14221 = VECTOR ( 'NONE', #917, 1000.000000000000000 ) ;
#14222 = DIRECTION ( 'NONE',  ( -0.9876526153536336894, -0.1566598588826349503, 0.000000000000000000 ) ) ;
#14223 = VERTEX_POINT ( 'NONE', #8048 ) ;
#14224 = DIRECTION ( 'NONE',  ( -0.1856185419698762329, 0.9826218788918640312, -0.000000000000000000 ) ) ;
#14225 = CIRCLE ( 'NONE', #6978, 42.89102435249441925 ) ;
#14226 = AXIS2_PLACEMENT_3D ( 'NONE', #16644, #432, #17798 ) ;
#14227 = EDGE_LOOP ( 'NONE', ( #13487, #17327 ) ) ;
#14228 = EDGE_CURVE ( 'NONE', #3396, #949, #17458, .T. ) ;
#14229 = EDGE_LOOP ( 'NONE', ( #7050, #40, #12994, #4686, #15626, #3537, #15148, #12915, #9920, #11419 ) ) ;
#14230 = DIRECTION ( 'NONE',  ( -0.9876526153536341335, -0.1566598588826327021, 0.000000000000000000 ) ) ;
#14231 = DIRECTION ( 'NONE',  ( 0.000000000000000000, 0.000000000000000000, 1.000000000000000000 ) ) ;
#14232 = VECTOR ( 'NONE', #15658, 1000.000000000000000 ) ;
#14233 = DIRECTION ( 'NONE',  ( 0.000000000000000000, 0.000000000000000000, 1.000000000000000000 ) ) ;
#14234 = AXIS2_PLACEMENT_3D ( 'NONE', #18560, #7064, #15757 ) ;
#14235 = VECTOR ( 'NONE', #6204, 1000.000000000000000 ) ;
#14236 = CONICAL_SURFACE ( 'NONE', #4228, 12.74754878398196567, 0.01745329251994333364 ) ;
#14237 = DIRECTION ( 'NONE',  ( -1.000000000000000000, 0.000000000000000000, 0.000000000000000000 ) ) ;
#14238 = FACE_BOUND ( 'NONE', #6162, .T. ) ;
#14239 = CARTESIAN_POINT ( 'NONE',  ( -35.67686938905902849, -25.90879301532540779, -12.99038105676658006 ) ) ;
#14240 = DIRECTION ( 'NONE',  ( -0.1566598588826321192, 0.9876526153536342445, 7.798540720466730171E-17 ) ) ;
#14241 = CARTESIAN_POINT ( 'NONE',  ( -3.373806069125576901, -15.72242466598909871, 4.330127018922213189 ) ) ;
#14242 = AXIS2_PLACEMENT_3D ( 'NONE', #6825, #5390, #7023 ) ;
#14243 = ADVANCED_FACE ( 'NONE', ( #15452 ), #18346, .F. ) ;
#14244 = CARTESIAN_POINT ( 'NONE',  ( -48.97054468615519340, -85.72288254658904805, 1.424741226644455312E-14 ) ) ;
#14245 = EDGE_CURVE ( 'NONE', #730, #14, #6860, .T. ) ;
#14246 = VERTEX_POINT ( 'NONE', #18630 ) ;
#14247 = CIRCLE ( 'NONE', #3609, 1.500000000000000888 ) ;
#14248 = EDGE_LOOP ( 'NONE', ( #4239, #17692 ) ) ;
#14249 = EDGE_CURVE ( 'NONE', #2390, #13318, #1121, .T. ) ;
#14250 = VERTEX_POINT ( 'NONE', #3680 ) ;
#14251 = ORIENTED_EDGE ( 'NONE', *, *, #15177, .F. ) ;
#14252 = CIRCLE ( 'NONE', #6212, 1.500000000000001332 ) ;
#14253 = DIRECTION ( 'NONE',  ( -0.9876526153536341335, -0.1566598588826327021, 0.000000000000000000 ) ) ;
#14254 = ORIENTED_EDGE ( 'NONE', *, *, #13307, .T. ) ;
#14255 = ORIENTED_EDGE ( 'NONE', *, *, #17865, .T. ) ;
#14256 = AXIS2_PLACEMENT_3D ( 'NONE', #18495, #17047, #4106 ) ;
#14257 = FACE_BOUND ( 'NONE', #12322, .T. ) ;
#14258 = AXIS2_PLACEMENT_3D ( 'NONE', #1726, #1124, #12639 ) ;
#14259 = AXIS2_PLACEMENT_3D ( 'NONE', #14920, #2027, #6413 ) ;
#14260 = LINE ( 'NONE', #15857, #7262 ) ;
#14261 = PRODUCT_DEFINITION_SHAPE ( 'NONE', 'NONE',  #18799 ) ;
#14262 = AXIS2_PLACEMENT_3D ( 'NONE', #12926, #17241, #2527 ) ;
#14263 = DIRECTION ( 'NONE',  ( -0.1566598588826321192, 0.9876526153536342445, 7.798540720466731404E-17 ) ) ;
#14264 = AXIS2_PLACEMENT_3D ( 'NONE', #10190, #17149, #4416 ) ;
#14265 = DIRECTION ( 'NONE',  ( -1.000000000000000000, 0.000000000000000000, 0.000000000000000000 ) ) ;
#14266 = ORIENTED_EDGE ( 'NONE', *, *, #3222, .T. ) ;
#14267 = EDGE_CURVE ( 'NONE', #5872, #1792, #14213, .T. ) ;
#14268 = LINE ( 'NONE', #136, #7875 ) ;
#14269 = CARTESIAN_POINT ( 'NONE',  ( -74.97862068226375243, -27.08026443497990243, -8.660254037844380193 ) ) ;
#14270 = ADVANCED_FACE ( 'NONE', ( #11263 ), #17081, .T. ) ;
#14271 = CARTESIAN_POINT ( 'NONE',  ( -3.578159390066044665, -20.81734760163988440, -17.32050807568878170 ) ) ;
#14272 = CIRCLE ( 'NONE', #9421, 1.500000000000000888 ) ;
#14273 = DIRECTION ( 'NONE',  ( -1.000000000000000000, 0.000000000000000000, 0.000000000000000000 ) ) ;
#14274 = EDGE_CURVE ( 'NONE', #13134, #7533, #5939, .T. ) ;
#14275 = EDGE_LOOP ( 'NONE', ( #17316, #17464, #15071, #1285 ) ) ;
#14276 = ORIENTED_EDGE ( 'NONE', *, *, #3876, .T. ) ;
#14277 = DIRECTION ( 'NONE',  ( 0.000000000000000000, 0.000000000000000000, 1.000000000000000000 ) ) ;
#14278 = CARTESIAN_POINT ( 'NONE',  ( -8.516422466834198346, -21.60064689605303911, 1.522258424776792809E-14 ) ) ;
#14279 = CIRCLE ( 'NONE', #15789, 5.000000000000000000 ) ;
#14280 = CIRCLE ( 'NONE', #10026, 1.500000000000001332 ) ;
#14281 = ORIENTED_EDGE ( 'NONE', *, *, #13149, .T. ) ;
#14282 = DIRECTION ( 'NONE',  ( -1.000000000000000000, 0.000000000000000000, 0.000000000000000000 ) ) ;
#14283 = ORIENTED_EDGE ( 'NONE', *, *, #12856, .T. ) ;
#14284 = DIRECTION ( 'NONE',  ( 0.000000000000000000, 0.000000000000000000, 1.000000000000000000 ) ) ;
#14285 = AXIS2_PLACEMENT_3D ( 'NONE', #6369, #16491, #863 ) ;
#14286 = DIRECTION ( 'NONE',  ( -0.1566598588826321747, 0.9876526153536343555, 0.000000000000000000 ) ) ;
#14287 = CIRCLE ( 'NONE', #1867, 1.499999999999999556 ) ;
#14288 = ORIENTED_EDGE ( 'NONE', *, *, #15308, .T. ) ;
#14289 = CARTESIAN_POINT ( 'NONE',  ( -41.39843176024032800, -21.75382923297043902, 21.65063509461102242 ) ) ;
#14290 = CARTESIAN_POINT ( 'NONE',  ( -58.84707083969148300, -87.28948113541537168, 8.660254037844412167 ) ) ;
#14291 = EDGE_LOOP ( 'NONE', ( #12540, #618 ) ) ;
#14292 = CARTESIAN_POINT ( 'NONE',  ( -21.81009776393036503, -81.41473642731668292, -12.99038105676658539 ) ) ;
#14293 = CARTESIAN_POINT ( 'NONE',  ( -25.26688191766805858, -81.96304593340589406, -4.330127018922185655 ) ) ;
#14294 = DIRECTION ( 'NONE',  ( 1.000000000000000000, 0.000000000000000000, 0.000000000000000000 ) ) ;
#14295 = ORIENTED_EDGE ( 'NONE', *, *, #15274, .T. ) ;
#14296 = AXIS2_PLACEMENT_3D ( 'NONE', #12647, #839, #5283 ) ;
#14297 = LINE ( 'NONE', #1328, #17304 ) ;
#14299 = ORIENTED_EDGE ( 'NONE', *, *, #7421, .T. ) ;
#14298 = LINE ( 'NONE', #1676, #15123 ) ;
#14300 = CIRCLE ( 'NONE', #17652, 5.000000000000004441 ) ;
#14301 = PLANE ( 'NONE',  #4238 ) ;
#14302 = ORIENTED_EDGE ( 'NONE', *, *, #8088, .F. ) ;
#14303 = ORIENTED_EDGE ( 'NONE', *, *, #10244, .T. ) ;
#14304 = EDGE_CURVE ( 'NONE', #13246, #11126, #10754, .T. ) ;
#14305 = AXIS2_PLACEMENT_3D ( 'NONE', #11558, #11728, #8916 ) ;
#14306 = EDGE_CURVE ( 'NONE', #1263, #11861, #3, .T. ) ;
#14307 = DIRECTION ( 'NONE',  ( -0.1566598588826321192, 0.9876526153536342445, 7.798540720466730171E-17 ) ) ;
#14308 = EDGE_LOOP ( 'NONE', ( #6431, #17661, #691, #1776 ) ) ;
#14309 = DIRECTION ( 'NONE',  ( -0.9876526153536341335, -0.1566598588826327021, 0.000000000000000000 ) ) ;
#14310 = AXIS2_PLACEMENT_3D ( 'NONE', #14990, #15079, #4658 ) ;
#14311 = ADVANCED_FACE ( 'NONE', ( #11622 ), #5691, .F. ) ;
#14312 = CARTESIAN_POINT ( 'NONE',  ( -57.36559191666103175, -87.05449134709142811, -8.660254037844385522 ) ) ;
#14313 = CARTESIAN_POINT ( 'NONE',  ( -49.59961335071796640, 37.20051552679456108, -20.00000000000000355 ) ) ;
#14314 = FACE_OUTER_BOUND ( 'NONE', #5670, .T. ) ;
#14315 = DIRECTION ( 'NONE',  ( 1.000000000000000000, 0.000000000000000000, -0.000000000000000000 ) ) ;
#14316 = EDGE_LOOP ( 'NONE', ( #14069, #9337 ) ) ;
#14317 = CARTESIAN_POINT ( 'NONE',  ( 55.85952145814821534, 6.938893903907228378E-15, 2.500000000000000000 ) ) ;
#14318 = CARTESIAN_POINT ( 'NONE',  ( -73.49714175923330117, -26.84527464665595886, 1.908195823574487804E-14 ) ) ;
#14319 = ORIENTED_EDGE ( 'NONE', *, *, #3693, .F. ) ;
#14320 = DIRECTION ( 'NONE',  ( 0.000000000000000000, 0.000000000000000000, 1.000000000000000000 ) ) ;
#14321 = DIRECTION ( 'NONE',  ( -0.1566598588826321192, 0.9876526153536342445, 7.798540720466730171E-17 ) ) ;
#14322 = EDGE_LOOP ( 'NONE', ( #18743, #7376 ) ) ;
#14323 = VERTEX_POINT ( 'NONE', #15831 ) ;
#14324 = DIRECTION ( 'NONE',  ( -0.1566598588826321192, 0.9876526153536342445, 7.798540720466730171E-17 ) ) ;
#14325 = AXIS2_PLACEMENT_3D ( 'NONE', #3120, #3202, #13437 ) ;
#14326 = ORIENTED_EDGE ( 'NONE', *, *, #14131, .F. ) ;
#14327 = CYLINDRICAL_SURFACE ( 'NONE', #15918, 1.500000000000001554 ) ;
#14328 = ORIENTED_EDGE ( 'NONE', *, *, #9903, .F. ) ;
#14329 = DIRECTION ( 'NONE',  ( -0.9876526153536341335, -0.1566598588826327021, 0.000000000000000000 ) ) ;
#14330 = FACE_BOUND ( 'NONE', #3708, .T. ) ;
#14331 = EDGE_CURVE ( 'NONE', #11762, #9117, #4417, .T. ) ;
#14332 = DIRECTION ( 'NONE',  ( 2.887450008416415878E-16, 0.000000000000000000, 1.000000000000000000 ) ) ;
#14333 = AXIS2_PLACEMENT_3D ( 'NONE', #16474, #5951, #259 ) ;
#14334 = DIRECTION ( 'NONE',  ( -0.1566598588826321192, 0.9876526153536342445, 7.798540720466730171E-17 ) ) ;
#14335 = EDGE_CURVE ( 'NONE', #6017, #12067, #2837, .T. ) ;
#14336 = ORIENTED_EDGE ( 'NONE', *, *, #5448, .F. ) ;
#14337 = LINE ( 'NONE', #7339, #1256 ) ;
#14338 = CARTESIAN_POINT ( 'NONE',  ( -68.72359699322777260, -88.85607972424168111, -17.32050807568878525 ) ) ;
#14339 = ORIENTED_EDGE ( 'NONE', *, *, #10421, .F. ) ;
#14340 = CARTESIAN_POINT ( 'NONE',  ( -70.04035760549561473, -26.29696514056674062, -17.32050807568878170 ) ) ;
#14341 = VERTEX_POINT ( 'NONE', #1429 ) ;
#14342 = VERTEX_POINT ( 'NONE', #11348 ) ;
#14343 = EDGE_LOOP ( 'NONE', ( #4566, #107 ) ) ;
#14344 = DIRECTION ( 'NONE',  ( -0.1566598588826321192, 0.9876526153536342445, 7.798540720466731404E-17 ) ) ;
#14345 = VECTOR ( 'NONE', #3650, 1000.000000000000000 ) ;
#14346 = ORIENTED_EDGE ( 'NONE', *, *, #13785, .T. ) ;
#14347 = FACE_BOUND ( 'NONE', #5174, .T. ) ;
#14348 = DIRECTION ( 'NONE',  ( -0.9876526153536336894, -0.1566598588826349503, 0.000000000000000000 ) ) ;
#14349 = ORIENTED_EDGE ( 'NONE', *, *, #4150, .T. ) ;
#14350 = EDGE_CURVE ( 'NONE', #610, #11762, #9936, .T. ) ;
#14351 = CARTESIAN_POINT ( 'NONE',  ( -66.25446545484369665, -88.46443007703511796, 12.99038105676661203 ) ) ;
#14352 = DIRECTION ( 'NONE',  ( -0.1566598588826321192, 0.9876526153536342445, 7.798540720466730171E-17 ) ) ;
#14353 = CARTESIAN_POINT ( 'NONE',  ( -76.88766983611584749, -2.536636612185957595, 25.00000000000000000 ) ) ;
#14354 = CONTEXT_DEPENDENT_SHAPE_REPRESENTATION ( #4226, #17141 ) ;
#14355 = EDGE_CURVE ( 'NONE', #18000, #15303, #13186, .T. ) ;
#14356 = VERTEX_POINT ( 'NONE', #2911 ) ;
#14357 = DIRECTION ( 'NONE',  ( -0.9876526153536336894, -0.1566598588826349503, 0.000000000000000000 ) ) ;
#14358 = FACE_BOUND ( 'NONE', #5944, .T. ) ;
#14359 = CARTESIAN_POINT ( 'NONE',  ( -62.00000000000000000, 0.000000000000000000, 20.00000000000001776 ) ) ;
#14360 = CARTESIAN_POINT ( 'NONE',  ( 0.000000000000000000, 0.000000000000000000, -25.00000000000000000 ) ) ;
#14361 = ORIENTED_EDGE ( 'NONE', *, *, #952, .F. ) ;
#14362 = ORIENTED_EDGE ( 'NONE', *, *, #5620, .F. ) ;
#14363 = DIRECTION ( 'NONE',  ( -0.9876526153536336894, -0.1566598588826349503, 0.000000000000000000 ) ) ;
#14364 = VERTEX_POINT ( 'NONE', #8712 ) ;
#14365 = DIRECTION ( 'NONE',  ( 0.000000000000000000, 0.000000000000000000, 1.000000000000000000 ) ) ;
#14366 = CARTESIAN_POINT ( 'NONE',  ( -55.22556837519115902, -23.94706725732727293, 1.908195823574487804E-14 ) ) ;
#14367 = ORIENTED_EDGE ( 'NONE', *, *, #18025, .F. ) ;
#14368 = EDGE_CURVE ( 'NONE', #9239, #16068, #18076, .T. ) ;
#14369 = ORIENTED_EDGE ( 'NONE', *, *, #7861, .T. ) ;
#14370 = ORIENTED_EDGE ( 'NONE', *, *, #2335, .F. ) ;
#14371 = CARTESIAN_POINT ( 'NONE',  ( -84.23462711737164454, 33.01666666666666572, 35.00000000000000000 ) ) ;
#14372 = CYLINDRICAL_SURFACE ( 'NONE', #9406, 1.500000000000001554 ) ;
#14373 = EDGE_CURVE ( 'NONE', #17705, #3775, #1615, .T. ) ;
#14374 = EDGE_CURVE ( 'NONE', #18673, #13460, #17446, .T. ) ;
#14375 = CARTESIAN_POINT ( 'NONE',  ( -126.1404785418517918, 9.595891400605990995, 2.500000000000000000 ) ) ;
#14376 = EDGE_CURVE ( 'NONE', #2561, #5872, #6559, .T. ) ;
#14377 = VECTOR ( 'NONE', #3309, 1000.000000000000227 ) ;
#14378 = LINE ( 'NONE', #8772, #6656 ) ;
#14379 = EDGE_CURVE ( 'NONE', #311, #7400, #13145, .T. ) ;
#14380 = DIRECTION ( 'NONE',  ( -0.9876526153536341335, -0.1566598588826327576, 0.000000000000000000 ) ) ;
#14381 = VERTEX_POINT ( 'NONE', #15726 ) ;
#14382 = CARTESIAN_POINT ( 'NONE',  ( -129.1404785418517918, -2.850701963179326892, -12.74754878398196389 ) ) ;
#14383 = FACE_OUTER_BOUND ( 'NONE', #11940, .T. ) ;
#14384 = LINE ( 'NONE', #16086, #1722 ) ;
#14385 = ORIENTED_EDGE ( 'NONE', *, *, #18305, .T. ) ;
#14386 = DIRECTION ( 'NONE',  ( 1.000000000000000000, 0.000000000000000000, 0.000000000000000000 ) ) ;
#14387 = CARTESIAN_POINT ( 'NONE',  ( -77.60964193335624373, -0.02405657537030136614, 4.939660022666148009 ) ) ;
#14389 = ORIENTED_EDGE ( 'NONE', *, *, #6436, .F. ) ;
#14388 = LINE ( 'NONE', #15893, #6039 ) ;
#14390 = ORIENTED_EDGE ( 'NONE', *, *, #1612, .F. ) ;
#14391 = DIRECTION ( 'NONE',  ( -0.1566598588826321192, 0.9876526153536342445, 7.798540720466730171E-17 ) ) ;
#14392 = CIRCLE ( 'NONE', #3465, 1.500000000000001332 ) ;
#14393 = CARTESIAN_POINT ( 'NONE',  ( -18.18859529943003750, -18.07232254922858417, 12.99038105676661381 ) ) ;
#14394 = VERTEX_POINT ( 'NONE', #5957 ) ;
#14395 = DIRECTION ( 'NONE',  ( -0.1566598588826321192, 0.9876526153536342445, 7.798540720466730171E-17 ) ) ;
#14396 = ADVANCED_FACE ( 'NONE', ( #11708 ), #17549, .F. ) ;
#14397 = DIRECTION ( 'NONE',  ( 0.000000000000000000, 0.000000000000000000, 1.000000000000000000 ) ) ;
#14398 = CARTESIAN_POINT ( 'NONE',  ( -85.13801595139509004, -33.83333333333328596, 100.5765140304660861 ) ) ;
#14399 = DIRECTION ( 'NONE',  ( -0.1566598588826321192, 0.9876526153536342445, 7.798540720466730171E-17 ) ) ;
#14400 = FACE_OUTER_BOUND ( 'NONE', #4489, .T. ) ;
#14401 = DIRECTION ( 'NONE',  ( 0.000000000000000000, 0.000000000000000000, 1.000000000000000000 ) ) ;
#14402 = DIRECTION ( 'NONE',  ( 1.000000000000000000, -0.000000000000000000, -0.000000000000000000 ) ) ;
#14403 = AXIS2_PLACEMENT_3D ( 'NONE', #12830, #16846, #12734 ) ;
#14404 = DIRECTION ( 'NONE',  ( -0.1566598588826321192, 0.9876526153536342445, 7.798540720466730171E-17 ) ) ;
#14405 = EDGE_CURVE ( 'NONE', #306, #17592, #8043, .T. ) ;
#14406 = DIRECTION ( 'NONE',  ( -0.9876526153536341335, -0.1566598588826327021, 0.000000000000000000 ) ) ;
#14408 = EDGE_LOOP ( 'NONE', ( #14088, #10426 ) ) ;
#14407 = DIRECTION ( 'NONE',  ( 0.9868632313631133801, -0.1615579233078772714, 2.999697980758352134E-17 ) ) ;
#14409 = DIRECTION ( 'NONE',  ( -0.9876526153536342445, -0.1566598588826321192, -3.168663947239273463E-17 ) ) ;
#14410 = ORIENTED_EDGE ( 'NONE', *, *, #5274, .F. ) ;
#14411 = EDGE_LOOP ( 'NONE', ( #1624, #10390, #9544, #8791, #4691, #10260 ) ) ;
#14412 = CARTESIAN_POINT ( 'NONE',  ( -70.24471092643608472, -31.39188807621751209, 4.330127018922217630 ) ) ;
#14413 = ORIENTED_EDGE ( 'NONE', *, *, #7990, .T. ) ;
#14414 = LINE ( 'NONE', #7230, #66 ) ;
#14415 = DIRECTION ( 'NONE',  ( -0.1566598588826321192, 0.9876526153536342445, 7.798540720466730171E-17 ) ) ;
#14416 = LINE ( 'NONE', #6763, #17271 ) ;
#14417 = EDGE_LOOP ( 'NONE', ( #17774, #14683, #10705, #826 ) ) ;
#14418 = FACE_BOUND ( 'NONE', #1817, .T. ) ;
#14419 = ADVANCED_FACE ( 'NONE', ( #1690 ), #7476, .F. ) ;
#14420 = ADVANCED_FACE ( 'NONE', ( #17166 ), #4149, .T. ) ;
#14421 = CARTESIAN_POINT ( 'NONE',  ( -55.42992169613162190, -29.04199019297804085, 4.330127018922217630 ) ) ;
#14422 = AXIS2_PLACEMENT_3D ( 'NONE', #11604, #11415, #4411 ) ;
#14423 = CARTESIAN_POINT ( 'NONE',  ( -6.995308533625909320, -79.06483854407721878, 4.330127018922213189 ) ) ;
#14424 = FACE_BOUND ( 'NONE', #9946, .T. ) ;
#14425 = CARTESIAN_POINT ( 'NONE',  ( -90.00000000000000000, 34.99999999999999289, 30.00000000000002487 ) ) ;
#14426 = EDGE_CURVE ( 'NONE', #4160, #4382, #4706, .T. ) ;
#14427 = CARTESIAN_POINT ( 'NONE',  ( -4.361458684479201153, -15.87908452487173427, -8.660254037844383745 ) ) ;
#14428 = ORIENTED_EDGE ( 'NONE', *, *, #9267, .F. ) ;
#14429 = EDGE_LOOP ( 'NONE', ( #13374, #11810 ) ) ;
#14430 = ORIENTED_EDGE ( 'NONE', *, *, #10801, .T. ) ;
#14431 = DIRECTION ( 'NONE',  ( -0.1566598588826321192, 0.9876526153536342445, 7.798540720466731404E-17 ) ) ;
#14432 = AXIS2_PLACEMENT_3D ( 'NONE', #13521, #1623, #16294 ) ;
#14433 = ORIENTED_EDGE ( 'NONE', *, *, #13722, .T. ) ;
#14434 = DIRECTION ( 'NONE',  ( 0.000000000000000000, 0.000000000000000000, -1.000000000000000000 ) ) ;
#14435 = DIRECTION ( 'NONE',  ( -0.1566598588826321747, 0.9876526153536343555, 0.000000000000000000 ) ) ;
#14436 = ORIENTED_EDGE ( 'NONE', *, *, #1740, .F. ) ;
#14437 = AXIS2_PLACEMENT_3D ( 'NONE', #3722, #9523, #5452 ) ;
#14438 = CIRCLE ( 'NONE', #7191, 1.499999999999999556 ) ;
#14439 = AXIS2_PLACEMENT_3D ( 'NONE', #17643, #15995, #3366 ) ;
#14440 = CARTESIAN_POINT ( 'NONE',  ( 0.000000000000000000, 0.000000000000000000, 30.00000000000000000 ) ) ;
#14441 = CARTESIAN_POINT ( 'NONE',  ( -75.18297400320422241, -32.17518737063066681, 12.99038105676661736 ) ) ;
#14442 = LINE ( 'NONE', #2957, #12998 ) ;
#14443 = CIRCLE ( 'NONE', #6290, 12.74754878398196567 ) ;
#14444 = CARTESIAN_POINT ( 'NONE',  ( -74.19532138785061193, -32.01852751174804013, 1.869203119972154228E-14 ) ) ;
#14445 = DIRECTION ( 'NONE',  ( 0.000000000000000000, 0.000000000000000000, 1.000000000000000000 ) ) ;
#14446 = FACE_OUTER_BOUND ( 'NONE', #16370, .T. ) ;
#14447 = CYLINDRICAL_SURFACE ( 'NONE', #6238, 2.200000000000000178 ) ;
#14448 = CARTESIAN_POINT ( 'NONE',  ( -54.73174206751433957, -23.86873732788595959, -4.330127018922180326 ) ) ;
#14449 = EDGE_LOOP ( 'NONE', ( #15121, #7431, #5669, #17228 ) ) ;
#14450 = VERTEX_POINT ( 'NONE', #1966 ) ;
#14451 = FACE_OUTER_BOUND ( 'NONE', #16321, .T. ) ;
#14452 = ADVANCED_FACE ( 'NONE', ( #4800 ), #14948, .F. ) ;
#14453 = AXIS2_PLACEMENT_3D ( 'NONE', #5551, #17037, #2694 ) ;
#14454 = AXIS2_PLACEMENT_3D ( 'NONE', #13969, #6697, #1021 ) ;
#14455 = AXIS2_PLACEMENT_3D ( 'NONE', #2119, #7906, #4672 ) ;
#14456 = CARTESIAN_POINT ( 'NONE',  ( -53.90880776292333820, -86.50618184100220276, -17.32050807568878525 ) ) ;
#14457 = CYLINDRICAL_SURFACE ( 'NONE', #13020, 1.500000000000001554 ) ;
#14458 = VERTEX_POINT ( 'NONE', #6159 ) ;
#14459 = CARTESIAN_POINT ( 'NONE',  ( -33.00338452973448966, -20.42222043246806962, 21.65063509461101887 ) ) ;
#14460 = EDGE_CURVE ( 'NONE', #14985, #6795, #10590, .T. ) ;
#14461 = VECTOR ( 'NONE', #4262, 1000.000000000000000 ) ;
#14462 = CARTESIAN_POINT ( 'NONE',  ( 0.000000000000000000, 0.000000000000000000, -30.00000000000000000 ) ) ;
#14463 = CARTESIAN_POINT ( 'NONE',  ( -18.18859529943003750, -18.07232254922857706, -21.65063509461098334 ) ) ;
#14464 = CIRCLE ( 'NONE', #17829, 1.500000000000000888 ) ;
#14465 = CYLINDRICAL_SURFACE ( 'NONE', #9351, 1.500000000000001554 ) ;
#14466 = DIRECTION ( 'NONE',  ( -0.9876526153536336894, -0.1566598588826349503, 0.000000000000000000 ) ) ;
#14467 = CARTESIAN_POINT ( 'NONE',  ( -8.312069145893737243, -16.50572396040226053, -21.65063509461098334 ) ) ;
#14468 = VERTEX_POINT ( 'NONE', #16195 ) ;
#14469 = CARTESIAN_POINT ( 'NONE',  ( -14.44233815895597672, -22.54060604934882051, -12.99038105676658006 ) ) ;
#14470 = AXIS2_PLACEMENT_3D ( 'NONE', #4623, #17732, #16112 ) ;
#14471 = EDGE_LOOP ( 'NONE', ( #12151, #18710, #1100, #9489 ) ) ;
#14473 = ORIENTED_EDGE ( 'NONE', *, *, #273, .T. ) ;
#14472 = DIRECTION ( 'NONE',  ( -0.1566598588826321747, 0.9876526153536343555, 0.000000000000000000 ) ) ;
#14474 = ADVANCED_FACE ( 'NONE', ( #3555 ), #18018, .F. ) ;
#14475 = AXIS2_PLACEMENT_3D ( 'NONE', #15860, #288, #6983 ) ;
#14476 = ADVANCED_FACE ( 'NONE', ( #15038 ), #10681, .F. ) ;
#14477 = DIRECTION ( 'NONE',  ( 0.000000000000000000, 0.000000000000000000, 1.000000000000000000 ) ) ;
#14478 = ORIENTED_EDGE ( 'NONE', *, *, #8806, .T. ) ;
#14479 = ADVANCED_FACE ( 'NONE', ( #4976 ), #9355, .F. ) ;
#14480 = ORIENTED_EDGE ( 'NONE', *, *, #8703, .T. ) ;
#14481 = DIRECTION ( 'NONE',  ( -1.000000000000000000, 1.224646799147353207E-16, 0.000000000000000000 ) ) ;
#14482 = ORIENTED_EDGE ( 'NONE', *, *, #7081, .T. ) ;
#14483 = DIRECTION ( 'NONE',  ( -0.1566598588826321192, 0.9876526153536342445, 7.798540720466731404E-17 ) ) ;
#14484 = FACE_OUTER_BOUND ( 'NONE', #10337, .T. ) ;
#14485 = CIRCLE ( 'NONE', #12634, 2.200000000000000178 ) ;
#14486 = ORIENTED_EDGE ( 'NONE', *, *, #10638, .F. ) ;
#14487 = CARTESIAN_POINT ( 'NONE',  ( -2.879979761448749009, -15.64409473654778893, -17.32050807568878170 ) ) ;
#14488 = CARTESIAN_POINT ( 'NONE',  ( -10.28737437660098131, -16.81904367816753165, -4.330127018922180326 ) ) ;
#14489 = CIRCLE ( 'NONE', #13263, 1.500000000000000888 ) ;
#14490 = CYLINDRICAL_SURFACE ( 'NONE', #9375, 1.500000000000001554 ) ;
#14491 = CARTESIAN_POINT ( 'NONE',  ( 55.85952145814821534, 6.938893903907228378E-15, 100.5765140304660861 ) ) ;
#14492 = AXIS2_PLACEMENT_3D ( 'NONE', #11189, #17013, #3985 ) ;
#14493 = ORIENTED_EDGE ( 'NONE', *, *, #7308, .F. ) ;
#14494 = CARTESIAN_POINT ( 'NONE',  ( -21.64537945316773460, -18.62063205531779886, 21.65063509461101532 ) ) ;
#14495 =( GEOMETRIC_REPRESENTATION_CONTEXT ( 3 ) GLOBAL_UNCERTAINTY_ASSIGNED_CONTEXT ( ( #2593 ) ) GLOBAL_UNIT_ASSIGNED_CONTEXT ( ( #7823, #16456, #16079 ) ) REPRESENTATION_CONTEXT ( 'NONE', 'WORKASPACE' ) );
#14496 = DIRECTION ( 'NONE',  ( -0.9876526153536336894, -0.1566598588826349503, 0.000000000000000000 ) ) ;
#14497 = DIRECTION ( 'NONE',  ( -0.1566598588826321747, 0.9876526153536343555, 0.000000000000000000 ) ) ;
#14498 = EDGE_CURVE ( 'NONE', #10091, #10067, #490, .T. ) ;
#14500 = ORIENTED_EDGE ( 'NONE', *, *, #14580, .T. ) ;
#14499 = DIRECTION ( 'NONE',  ( -0.1566598588826321747, 0.9876526153536343555, 0.000000000000000000 ) ) ;
#14502 = ORIENTED_EDGE ( 'NONE', *, *, #10746, .T. ) ;
#14501 = EDGE_CURVE ( 'NONE', #13816, #1601, #7763, .T. ) ;
#14503 = CARTESIAN_POINT ( 'NONE',  ( -59.38053215754616332, -29.66862962850856533, -17.32050807568878170 ) ) ;
#14504 = AXIS2_PLACEMENT_3D ( 'NONE', #18739, #12708, #18563 ) ;
#14505 = ORIENTED_EDGE ( 'NONE', *, *, #812, .F. ) ;
#14506 = ORIENTED_EDGE ( 'NONE', *, *, #12149, .F. ) ;
#14507 = CYLINDRICAL_SURFACE ( 'NONE', #8052, 1.500000000000000666 ) ;
#14508 = VECTOR ( 'NONE', #15320, 1000.000000000000000 ) ;
#14509 = EDGE_CURVE ( 'NONE', #719, #8415, #8960, .T. ) ;
#14510 = VECTOR ( 'NONE', #7221, 1000.000000000000000 ) ;
#14511 = DIRECTION ( 'NONE',  ( 0.9876526153536342445, 0.1566598588826321192, 0.000000000000000000 ) ) ;
#14512 = ORIENTED_EDGE ( 'NONE', *, *, #14539, .T. ) ;
#14513 = CARTESIAN_POINT ( 'NONE',  ( -76.98587034812761942, -1.614196834991422858, -6.560995283100326425 ) ) ;
#14514 = CIRCLE ( 'NONE', #8755, 1.500000000000000888 ) ;
#14515 = CIRCLE ( 'NONE', #11167, 1.500000000000000888 ) ;
#14516 = FACE_OUTER_BOUND ( 'NONE', #1111, .T. ) ;
#14517 = VERTEX_POINT ( 'NONE', #17931 ) ;
#14518 = AXIS2_PLACEMENT_3D ( 'NONE', #14928, #3627, #9433 ) ;
#14519 = SURFACE_STYLE_USAGE ( .BOTH. , #13365 ) ;
#14520 = VERTEX_POINT ( 'NONE', #10395 ) ;
#14521 = DIRECTION ( 'NONE',  ( 1.000000000000000000, 0.000000000000000000, 0.000000000000000000 ) ) ;
#14522 = CIRCLE ( 'NONE', #6364, 1.500000000000000888 ) ;
#14523 = AXIS2_PLACEMENT_3D ( 'NONE', #7146, #4561, #3129 ) ;
#14524 = DIRECTION ( 'NONE',  ( -0.000000000000000000, -0.000000000000000000, -1.000000000000000000 ) ) ;
#14525 = CYLINDRICAL_SURFACE ( 'NONE', #3897, 1.500000000000001554 ) ;
#14526 = FACE_BOUND ( 'NONE', #6778, .T. ) ;
#14527 = DIRECTION ( 'NONE',  ( -0.1566598588826321192, 0.9876526153536342445, 7.798540720466731404E-17 ) ) ;
#14528 = EDGE_LOOP ( 'NONE', ( #876, #15651, #14951, #18332 ) ) ;
#14529 = ORIENTED_EDGE ( 'NONE', *, *, #17656, .T. ) ;
#14530 = TOROIDAL_SURFACE ( 'NONE', #5447, 3.000000000000000000, 2.000000000000000000 ) ;
#14531 = VERTEX_POINT ( 'NONE', #3462 ) ;
#14532 = CARTESIAN_POINT ( 'NONE',  ( -38.14600092744309734, -26.30044266253198160, 1.175313729581431390E-14 ) ) ;
#14533 = VERTEX_POINT ( 'NONE', #8974 ) ;
#14534 = VECTOR ( 'NONE', #3065, 1000.000000000000000 ) ;
#14535 = FACE_BOUND ( 'NONE', #7741, .T. ) ;
#14536 = ADVANCED_FACE ( 'NONE', ( #2160 ), #4897, .F. ) ;
#14537 = CARTESIAN_POINT ( 'NONE',  ( -3.538524379888208227, -78.51652903798800764, 12.99038105676660848 ) ) ;
#14538 = AXIS2_PLACEMENT_3D ( 'NONE', #18758, #10442, #10537 ) ;
#14539 = EDGE_CURVE ( 'NONE', #8813, #16572, #17470, .T. ) ;
#14540 = ORIENTED_EDGE ( 'NONE', *, *, #2559, .F. ) ;
#14541 = ADVANCED_FACE ( 'NONE', ( #457 ), #9883, .T. ) ;
#14542 = CONTEXT_DEPENDENT_SHAPE_REPRESENTATION ( #10142, #4974 ) ;
#14543 = ORIENTED_EDGE ( 'NONE', *, *, #15297, .F. ) ;
#14544 = CARTESIAN_POINT ( 'NONE',  ( -174.0603277000674325, 56.10099541002031742, 3.279750847804461245 ) ) ;
#14546 = CARTESIAN_POINT ( 'NONE',  ( -88.14047854185180597, -33.59999999999994458, -24.99999999999999645 ) ) ;
#14545 = AXIS2_PLACEMENT_3D ( 'NONE', #18652, #4179, #9964 ) ;
#14547 = CARTESIAN_POINT ( 'NONE',  ( -70.11841833929642576, 45.05038753831868803, -6.363771460920504275 ) ) ;
#14548 = AXIS2_PLACEMENT_3D ( 'NONE', #5021, #12603, #9501 ) ;
#14549 = DIRECTION ( 'NONE',  ( -1.000000000000000000, -0.000000000000000000, -0.000000000000000000 ) ) ;
#14550 = ORIENTED_EDGE ( 'NONE', *, *, #8815, .F. ) ;
#14551 = EDGE_LOOP ( 'NONE', ( #5375, #9601 ) ) ;
#14552 = CARTESIAN_POINT ( 'NONE',  ( -8.312069145893737243, -16.50572396040226053, 4.330127018922214965 ) ) ;
#14553 = DIRECTION ( 'NONE',  ( -0.9876526153536336894, -0.1566598588826349503, 0.000000000000000000 ) ) ;
#14554 = ORIENTED_EDGE ( 'NONE', *, *, #13342, .T. ) ;
#14555 = EDGE_LOOP ( 'NONE', ( #13709, #7352, #11970, #9316 ) ) ;
#14556 = CARTESIAN_POINT ( 'NONE',  ( -57.85941822433786541, -87.13282127653275211, 12.99038105676661203 ) ) ;
#14557 = FACE_BOUND ( 'NONE', #1013, .T. ) ;
#14558 = EDGE_CURVE ( 'NONE', #6040, #17749, #9272, .T. ) ;
#14559 = DIRECTION ( 'NONE',  ( 0.000000000000000000, 0.000000000000000000, 1.000000000000000000 ) ) ;
#14560 = AXIS2_PLACEMENT_3D ( 'NONE', #8947, #1582, #6019 ) ;
#14561 = ORIENTED_EDGE ( 'NONE', *, *, #10177, .T. ) ;
#14562 = DIRECTION ( 'NONE',  ( -0.1566598588826321747, 0.9876526153536343555, 0.000000000000000000 ) ) ;
#14563 = CARTESIAN_POINT ( 'NONE',  ( -79.91688375903190433, -27.86356372939306425, 1.908195823574487804E-14 ) ) ;
#14564 = EDGE_CURVE ( 'NONE', #12921, #13088, #4426, .T. ) ;
#14565 = VECTOR ( 'NONE', #10674, 1000.000000000000227 ) ;
#14566 = CARTESIAN_POINT ( 'NONE',  ( -10.94591899504043830, -79.69147797960773971, -17.32050807568878525 ) ) ;
#14567 = DIRECTION ( 'NONE',  ( 1.000000000000000000, 0.000000000000000000, 0.000000000000000000 ) ) ;
#14568 = ORIENTED_EDGE ( 'NONE', *, *, #5125, .F. ) ;
#14569 = DIRECTION ( 'NONE',  ( -0.1566598588826321747, 0.9876526153536343555, 0.000000000000000000 ) ) ;
#14570 = ORIENTED_EDGE ( 'NONE', *, *, #11353, .T. ) ;
#14571 = AXIS2_PLACEMENT_3D ( 'NONE', #5629, #2678, #1458 ) ;
#14572 = ORIENTED_EDGE ( 'NONE', *, *, #5661, .T. ) ;
#14573 = ORIENTED_EDGE ( 'NONE', *, *, #16560, .F. ) ;
#14574 = VECTOR ( 'NONE', #4866, 1000.000000000000000 ) ;
#14575 = ORIENTED_EDGE ( 'NONE', *, *, #16610, .T. ) ;
#14576 = LINE ( 'NONE', #6236, #15039 ) ;
#14577 = VECTOR ( 'NONE', #5681, 1000.000000000000000 ) ;
#14578 = AXIS2_PLACEMENT_3D ( 'NONE', #995, #6766, #5133 ) ;
#14579 = CARTESIAN_POINT ( 'NONE',  ( -131.1404785418517918, -2.850701963179326892, 13.78215425775057845 ) ) ;
#14580 = EDGE_CURVE ( 'NONE', #1802, #10598, #1881, .T. ) ;
#14581 = CARTESIAN_POINT ( 'NONE',  ( -56.91140061916208026, -29.27697998130198442, 4.330127018922217630 ) ) ;
#14582 = VERTEX_POINT ( 'NONE', #13509 ) ;
#14583 = FACE_OUTER_BOUND ( 'NONE', #14449, .T. ) ;
#14584 = DIRECTION ( 'NONE',  ( -0.1566598588826321192, 0.9876526153536342445, 7.798540720466730171E-17 ) ) ;
#14585 = FACE_OUTER_BOUND ( 'NONE', #18786, .T. ) ;
#14586 = VECTOR ( 'NONE', #2907, 1000.000000000000000 ) ;
#14587 = CARTESIAN_POINT ( 'NONE',  ( -129.1404785418517918, -2.850701963179328668, 12.74754878398196745 ) ) ;
#14588 = DIRECTION ( 'NONE',  ( -0.1566598588826321192, 0.9876526153536342445, 7.798540720466730171E-17 ) ) ;
#14589 = ADVANCED_FACE ( 'NONE', ( #16781 ), #9457, .F. ) ;
#14590 = CARTESIAN_POINT ( 'NONE',  ( 0.000000000000000000, 0.000000000000000000, -30.00000000000000000 ) ) ;
#14591 = DIRECTION ( 'NONE',  ( -0.1566598588826321192, 0.9876526153536342445, 7.798540720466731404E-17 ) ) ;
#14592 = DIRECTION ( 'NONE',  ( 1.000000000000000000, 0.000000000000000000, 0.000000000000000000 ) ) ;
#14593 = EDGE_CURVE ( 'NONE', #5983, #7813, #14000, .T. ) ;
#14594 = ORIENTED_EDGE ( 'NONE', *, *, #12905, .T. ) ;
#14595 = AXIS2_PLACEMENT_3D ( 'NONE', #16334, #16438, #10261 ) ;
#14596 = VERTEX_POINT ( 'NONE', #746 ) ;
#14597 = LINE ( 'NONE', #10222, #5967 ) ;
#14598 = ORIENTED_EDGE ( 'NONE', *, *, #9879, .T. ) ;
#14599 = VERTEX_POINT ( 'NONE', #1050 ) ;
#14600 = CARTESIAN_POINT ( 'NONE',  ( -47.32434745236212592, -22.69378838626621686, -17.32050807568878170 ) ) ;
#14601 = CIRCLE ( 'NONE', #2174, 2.200000000000000178 ) ;
#14602 = EDGE_LOOP ( 'NONE', ( #14771, #13880, #13167, #9695 ) ) ;
#14603 = PLANE ( 'NONE',  #17641 ) ;
#14604 = ORIENTED_EDGE ( 'NONE', *, *, #14709, .T. ) ;
#14605 = DIRECTION ( 'NONE',  ( -0.1566598588826321192, 0.9876526153536342445, 7.798540720466730171E-17 ) ) ;
#14606 = PLANE ( 'NONE',  #3697 ) ;
#14607 = CARTESIAN_POINT ( 'NONE',  ( -79.50968810220766159, 31.87664632526870889, -35.00000000000000000 ) ) ;
#14608 = EDGE_CURVE ( 'NONE', #6818, #10150, #12272, .T. ) ;
#14609 = ADVANCED_FACE ( 'NONE', ( #9832 ), #5384, .F. ) ;
#14610 = ADVANCED_FACE ( 'NONE', ( #15598 ), #8232, .F. ) ;
#14611 = DIRECTION ( 'NONE',  ( 0.000000000000000000, 0.000000000000000000, 1.000000000000000000 ) ) ;
#14612 = VERTEX_POINT ( 'NONE', #11139 ) ;
#14613 = SURFACE_STYLE_FILL_AREA ( #11638 ) ;
#14614 = ORIENTED_EDGE ( 'NONE', *, *, #3653, .F. ) ;
#14615 = AXIS2_PLACEMENT_3D ( 'NONE', #7794, #14802, #6199 ) ;
#14616 = DIRECTION ( 'NONE',  ( 0.000000000000000000, 0.000000000000000000, 1.000000000000000000 ) ) ;
#14617 = DIRECTION ( 'NONE',  ( -0.9876526153536344665, -0.1566598588826304539, 0.000000000000000000 ) ) ;
#14618 = DIRECTION ( 'NONE',  ( -0.9876526153536336894, -0.1566598588826349503, 0.000000000000000000 ) ) ;
#14619 = CARTESIAN_POINT ( 'NONE',  ( -63.82496892663746735, -30.37359899348040315, -21.65063509461098334 ) ) ;
#14620 = VERTEX_POINT ( 'NONE', #2337 ) ;
#14621 = ORIENTED_EDGE ( 'NONE', *, *, #4644, .T. ) ;
#14622 = ORIENTED_EDGE ( 'NONE', *, *, #5419, .F. ) ;
#14623 = ORIENTED_EDGE ( 'NONE', *, *, #17924, .T. ) ;
#14624 = DIRECTION ( 'NONE',  ( -0.1566598588826321192, 0.9876526153536342445, 7.798540720466731404E-17 ) ) ;
#14625 = EDGE_LOOP ( 'NONE', ( #9019, #18569 ) ) ;
#14626 = CARTESIAN_POINT ( 'NONE',  ( -175.0988807681447383, 56.35851375132025254, 2.556294622946508611E-15 ) ) ;
#14627 = VERTEX_POINT ( 'NONE', #946 ) ;
#14628 = CARTESIAN_POINT ( 'NONE',  ( -3.000000000000004441, 0.000000000000000000, -20.00000000000000355 ) ) ;
#14629 = ORIENTED_EDGE ( 'NONE', *, *, #16052, .F. ) ;
#14630 = AXIS2_PLACEMENT_3D ( 'NONE', #6741, #8144, #4989 ) ;
#14631 = ORIENTED_EDGE ( 'NONE', *, *, #5189, .F. ) ;
#14632 = DIRECTION ( 'NONE',  ( -0.1566598588826321747, 0.9876526153536343555, 0.000000000000000000 ) ) ;
#14633 = CARTESIAN_POINT ( 'NONE',  ( -40.08167114797252140, -84.31294381664535820, -21.65063509461098690 ) ) ;
#14634 = LINE ( 'NONE', #4305, #2418 ) ;
#14635 = CARTESIAN_POINT ( 'NONE',  ( 3.231158466157554976, 19.73726462726228092, 24.99999999999999289 ) ) ;
#14636 = EDGE_CURVE ( 'NONE', #11597, #16602, #6620, .T. ) ;
#14637 = CARTESIAN_POINT ( 'NONE',  ( -174.8836357390702005, 55.21905606219750240, -5.316127001577088507 ) ) ;
#14638 = CARTESIAN_POINT ( 'NONE',  ( -29.75095369693726610, -24.96883386202961574, 8.660254037844417496 ) ) ;
#14639 = EDGE_LOOP ( 'NONE', ( #13730, #7242, #16053, #1983 ) ) ;
#14640 = EDGE_CURVE ( 'NONE', #886, #4810, #11074, .T. ) ;
#14641 = EDGE_LOOP ( 'NONE', ( #8419, #5466 ) ) ;
#14642 = AXIS2_PLACEMENT_3D ( 'NONE', #1337, #1515, #17359 ) ;
#14643 = LINE ( 'NONE', #6308, #5077 ) ;
#14644 = EDGE_LOOP ( 'NONE', ( #1999, #1500 ) ) ;
#14645 = CARTESIAN_POINT ( 'NONE',  ( 1.360103686702108128, -20.03404830722672259, 1.348786077179111942E-14 ) ) ;
#14646 = DIRECTION ( 'NONE',  ( -0.9876526153536341335, -0.1566598588826327021, 0.000000000000000000 ) ) ;
#14647 = VERTEX_POINT ( 'NONE', #6913 ) ;
#14648 = ORIENTED_EDGE ( 'NONE', *, *, #16453, .T. ) ;
#14649 = DIRECTION ( 'NONE',  ( -0.000000000000000000, -0.000000000000000000, 1.000000000000000000 ) ) ;
#14650 = CARTESIAN_POINT ( 'NONE',  ( -47.48906576312474215, -85.48789275826510448, 1.443110928631665584E-14 ) ) ;
#14651 = CARTESIAN_POINT ( 'NONE',  ( -16.87183468716221313, -80.63143713290354242, 21.65063509461101532 ) ) ;
#14652 = DIRECTION ( 'NONE',  ( -0.1566598588826321192, 0.9876526153536342445, 7.798540720466730171E-17 ) ) ;
#14653 = ADVANCED_FACE ( 'NONE', ( #842 ), #10853, .F. ) ;
#14654 = DIRECTION ( 'NONE',  ( -0.1566598588826321747, 0.9876526153536343555, 0.000000000000000000 ) ) ;
#14655 = CARTESIAN_POINT ( 'NONE',  ( -65.30644784966793281, -30.60858878180435738, -12.99038105676658006 ) ) ;
#14656 = ORIENTED_EDGE ( 'NONE', *, *, #8530, .F. ) ;
#14657 = ORIENTED_EDGE ( 'NONE', *, *, #5520, .T. ) ;
#14658 = DIRECTION ( 'NONE',  ( -0.000000000000000000, -0.000000000000000000, -1.000000000000000000 ) ) ;
#14659 = ORIENTED_EDGE ( 'NONE', *, *, #6674, .T. ) ;
#14660 = EDGE_CURVE ( 'NONE', #16376, #11672, #11372, .T. ) ;
#14661 = DIRECTION ( 'NONE',  ( -0.1566598588826321747, 0.9876526153536343555, 0.000000000000000000 ) ) ;
#14662 = VERTEX_POINT ( 'NONE', #16869 ) ;
#14663 = ORIENTED_EDGE ( 'NONE', *, *, #5216, .T. ) ;
#14664 = CIRCLE ( 'NONE', #4669, 1.500000000000000000 ) ;
#14665 = FACE_OUTER_BOUND ( 'NONE', #3319, .T. ) ;
#14666 = CARTESIAN_POINT ( 'NONE',  ( -55.42992169613163611, -29.04199019297804085, -4.330127018922181215 ) ) ;
#14667 = CARTESIAN_POINT ( 'NONE',  ( -56.37793930130741415, -86.89783148820879433, -21.65063509461098690 ) ) ;
#14668 = FACE_OUTER_BOUND ( 'NONE', #7621, .T. ) ;
#14669 = CYLINDRICAL_SURFACE ( 'NONE', #10335, 1.500000000000001554 ) ;
#14670 = CARTESIAN_POINT ( 'NONE',  ( -86.18478963674542115, 32.34879426031891114, 35.00000000000000000 ) ) ;
#14671 = CARTESIAN_POINT ( 'NONE',  ( -42.38608437559395270, -21.91048909185307281, 17.32050807568881723 ) ) ;
#14672 = DIRECTION ( 'NONE',  ( -0.1566598588826321192, 0.9876526153536342445, 7.798540720466730171E-17 ) ) ;
#14673 = DIRECTION ( 'NONE',  ( 0.000000000000000000, 0.000000000000000000, 1.000000000000000000 ) ) ;
#14674 = DIRECTION ( 'NONE',  ( -0.9876526153536341335, -0.1566598588826327021, 0.000000000000000000 ) ) ;
#14675 = AXIS2_PLACEMENT_3D ( 'NONE', #3165, #14741, #1758 ) ;
#14677 = ORIENTED_EDGE ( 'NONE', *, *, #2828, .T. ) ;
#14676 = DIRECTION ( 'NONE',  ( 0.9539392014169441047, 0.3000000000000045963, -2.548423110585629762E-16 ) ) ;
#14678 = ORIENTED_EDGE ( 'NONE', *, *, #489, .T. ) ;
#14679 = EDGE_LOOP ( 'NONE', ( #18369, #5673, #4317, #4357 ) ) ;
#14680 = DIRECTION ( 'NONE',  ( -0.1566598588826321192, 0.9876526153536342445, 7.798540720466730171E-17 ) ) ;
#14681 = ORIENTED_EDGE ( 'NONE', *, *, #14068, .T. ) ;
#14682 = ADVANCED_FACE ( 'NONE', ( #3655 ), #18223, .F. ) ;
#14683 = ORIENTED_EDGE ( 'NONE', *, *, #2864, .T. ) ;
#14684 = VERTEX_POINT ( 'NONE', #3835 ) ;
#14685 = CARTESIAN_POINT ( 'NONE',  ( 1.360103686702108128, -20.03404830722672259, -8.660254037844383745 ) ) ;
#14686 = FACE_OUTER_BOUND ( 'NONE', #5827, .T. ) ;
#14687 = EDGE_CURVE ( 'NONE', #17456, #697, #3198, .T. ) ;
#14688 = CARTESIAN_POINT ( 'NONE',  ( -3.578159390066044665, -20.81734760163988440, 17.32050807568881012 ) ) ;
#14689 = FACE_OUTER_BOUND ( 'NONE', #13025, .T. ) ;
#14690 = CARTESIAN_POINT ( 'NONE',  ( -343.6658356661351945, -4.573248343763018475, 9.951701414186830458E-16 ) ) ;
#14691 = LINE ( 'NONE', #9199, #8139 ) ;
#14692 = EDGE_LOOP ( 'NONE', ( #13260, #521 ) ) ;
#14693 = PLANE ( 'NONE',  #15198 ) ;
#14694 = ORIENTED_EDGE ( 'NONE', *, *, #7223, .F. ) ;
#14695 = AXIS2_PLACEMENT_3D ( 'NONE', #678, #2264, #15347 ) ;
#14696 = CARTESIAN_POINT ( 'NONE',  ( -6.047290928450125946, -21.20899724884646531, 4.330127018922214077 ) ) ;
#14697 = EDGE_CURVE ( 'NONE', #8575, #8619, #5651, .T. ) ;
#14698 = CARTESIAN_POINT ( 'NONE',  ( -35.63723437888118184, -83.60797445167352748, 8.660254037844412167 ) ) ;
#14699 = VECTOR ( 'NONE', #14672, 1000.000000000000000 ) ;
#14700 = VERTEX_POINT ( 'NONE', #16970 ) ;
#14701 = ORIENTED_EDGE ( 'NONE', *, *, #14705, .T. ) ;
#14702 = ORIENTED_EDGE ( 'NONE', *, *, #14813, .T. ) ;
#14703 = VERTEX_POINT ( 'NONE', #9754 ) ;
#14704 = FACE_OUTER_BOUND ( 'NONE', #3156, .T. ) ;
#14705 = EDGE_CURVE ( 'NONE', #10784, #11150, #14115, .T. ) ;
#14706 = EDGE_CURVE ( 'NONE', #16580, #15439, #12587, .T. ) ;
#14707 = ORIENTED_EDGE ( 'NONE', *, *, #11287, .T. ) ;
#14708 = FACE_BOUND ( 'NONE', #7840, .T. ) ;
#14709 = EDGE_CURVE ( 'NONE', #14890, #10439, #2906, .T. ) ;
#14710 = DIRECTION ( 'NONE',  ( 0.000000000000000000, 0.000000000000000000, 1.000000000000000000 ) ) ;
#14711 = TOROIDAL_SURFACE ( 'NONE', #4113, 13.78215425775057668, 2.000000000000000000 ) ;
#14712 = DIRECTION ( 'NONE',  ( -0.1566598588826321192, 0.9876526153536342445, 7.798540720466731404E-17 ) ) ;
#14713 = ORIENTED_EDGE ( 'NONE', *, *, #757, .F. ) ;
#14714 = ORIENTED_EDGE ( 'NONE', *, *, #10612, .F. ) ;
#14715 = CARTESIAN_POINT ( 'NONE',  ( -37.44782129882580080, -21.12718979743991454, 17.32050807568881723 ) ) ;
#14716 = DIRECTION ( 'NONE',  ( -0.1566598588826321192, 0.9876526153536342445, 7.798540720466731404E-17 ) ) ;
#14717 = CARTESIAN_POINT ( 'NONE',  ( -37.44782129882580080, -21.12718979743988967, 1.232676135170975081E-14 ) ) ;
#14718 = DIRECTION ( 'NONE',  ( 0.000000000000000000, 0.000000000000000000, 1.000000000000000000 ) ) ;
#14719 = VERTEX_POINT ( 'NONE', #5575 ) ;
#14720 = VERTEX_POINT ( 'NONE', #5774 ) ;
#14721 = LINE ( 'NONE', #620, #12334 ) ;
#14722 = VECTOR ( 'NONE', #10894, 1000.000000000000000 ) ;
#14723 = CARTESIAN_POINT ( 'NONE',  ( 0.000000000000000000, 0.000000000000000000, 30.00000000000000000 ) ) ;
#14724 = ADVANCED_FACE ( 'NONE', ( #7015 ), #7108, .F. ) ;
#14725 = CARTESIAN_POINT ( 'NONE',  ( -52.92115514756972061, -86.34952198211958319, -12.99038105676658539 ) ) ;
#14726 = EDGE_CURVE ( 'NONE', #16165, #9184, #10287, .T. ) ;
#14727 = EDGE_CURVE ( 'NONE', #384, #13798, #13203, .T. ) ;
#14728 = AXIS2_PLACEMENT_3D ( 'NONE', #16280, #6247, #16391 ) ;
#14729 = ORIENTED_EDGE ( 'NONE', *, *, #8730, .F. ) ;
#14730 = DIRECTION ( 'NONE',  ( -0.1566598588826321747, 0.9876526153536343555, 0.000000000000000000 ) ) ;
#14731 = DIRECTION ( 'NONE',  ( 8.693966348389027220E-17, -1.991237296706374949E-16, 1.000000000000000000 ) ) ;
#14732 = EDGE_CURVE ( 'NONE', #11672, #16376, #13489, .T. ) ;
#14733 = VECTOR ( 'NONE', #16240, 1000.000000000000000 ) ;
#14734 = FACE_OUTER_BOUND ( 'NONE', #1305, .T. ) ;
#14735 = CIRCLE ( 'NONE', #17186, 1.500000000000000000 ) ;
#14736 = DIRECTION ( 'NONE',  ( -0.9876526153536341335, -0.1566598588826327021, 0.000000000000000000 ) ) ;
#14737 = DIRECTION ( 'NONE',  ( -0.1566598588826321192, 0.9876526153536342445, 7.798540720466730171E-17 ) ) ;
#14738 = AXIS2_PLACEMENT_3D ( 'NONE', #6325, #6136, #4956 ) ;
#14739 = DIRECTION ( 'NONE',  ( -0.000000000000000000, -0.000000000000000000, -1.000000000000000000 ) ) ;
#14740 = AXIS2_PLACEMENT_3D ( 'NONE', #1699, #17662, #1887 ) ;
#14741 = DIRECTION ( 'NONE',  ( -0.1566598588826321192, 0.9876526153536342445, 7.798540720466731404E-17 ) ) ;
#14742 = DIRECTION ( 'NONE',  ( -0.1566598588826321192, 0.9876526153536342445, 7.798540720466730171E-17 ) ) ;
#14743 = VERTEX_POINT ( 'NONE', #12759 ) ;
#14744 = ORIENTED_EDGE ( 'NONE', *, *, #3923, .T. ) ;
#14745 = CARTESIAN_POINT ( 'NONE',  ( 0.000000000000000000, 0.000000000000000000, 35.00000000000000000 ) ) ;
#14746 = ORIENTED_EDGE ( 'NONE', *, *, #3269, .T. ) ;
#14747 = VERTEX_POINT ( 'NONE', #4328 ) ;
#14748 = AXIS2_PLACEMENT_3D ( 'NONE', #1055, #17256, #18323 ) ;
#14749 = ORIENTED_EDGE ( 'NONE', *, *, #13875, .T. ) ;
#14750 = AXIS2_PLACEMENT_3D ( 'NONE', #4952, #8092, #5050 ) ;
#14751 = DIRECTION ( 'NONE',  ( -0.9876526153536341335, -0.1566598588826327021, 0.000000000000000000 ) ) ;
#14752 = EDGE_CURVE ( 'NONE', #1621, #18515, #16234, .T. ) ;
#14753 = AXIS2_PLACEMENT_3D ( 'NONE', #18469, #5432, #8187 ) ;
#14754 = CARTESIAN_POINT ( 'NONE',  ( -90.00000000000000000, 34.99999999999999289, -30.00000000000000000 ) ) ;
#14755 = EDGE_CURVE ( 'NONE', #16874, #11180, #10100, .T. ) ;
#14756 = CARTESIAN_POINT ( 'NONE',  ( -61.15148406731293562, -24.88702641062305787, -12.99038105676658006 ) ) ;
#14757 = CARTESIAN_POINT ( 'NONE',  ( 11.59211860341528144, 6.314490184041265053, -130.3485206753969976 ) ) ;
#14758 = CARTESIAN_POINT ( 'NONE',  ( -5.513829610595458064, -78.82984875575326100, -4.330127018922185655 ) ) ;
#14759 = DIRECTION ( 'NONE',  ( 1.000000000000000000, 0.000000000000000000, 0.000000000000000000 ) ) ;
#14760 = VERTEX_POINT ( 'NONE', #17145 ) ;
#14761 = EDGE_CURVE ( 'NONE', #2452, #1415, #8056, .T. ) ;
#14762 = VECTOR ( 'NONE', #11623, 1000.000000000000000 ) ;
#14763 = DIRECTION ( 'NONE',  ( -0.1566598588826321747, 0.9876526153536343555, 0.000000000000000000 ) ) ;
#14764 = VERTEX_POINT ( 'NONE', #1230 ) ;
#14765 = CARTESIAN_POINT ( 'NONE',  ( -36.46016868347218320, -20.97052993855727721, 12.99038105676661736 ) ) ;
#14766 = LINE ( 'NONE', #5, #6317 ) ;
#14767 = DIRECTION ( 'NONE',  ( -0.9876526153536344665, -0.1566598588826304539, 0.000000000000000000 ) ) ;
#14768 = VERTEX_POINT ( 'NONE', #5858 ) ;
#14769 = EDGE_LOOP ( 'NONE', ( #10623, #11360 ) ) ;
#14770 = CIRCLE ( 'NONE', #17516, 1.499999999999997335 ) ;
#14771 = ORIENTED_EDGE ( 'NONE', *, *, #15365, .F. ) ;
#14772 = DIRECTION ( 'NONE',  ( -1.000000000000000000, -0.000000000000000000, -0.000000000000000000 ) ) ;
#14773 = ORIENTED_EDGE ( 'NONE', *, *, #10396, .T. ) ;
#14774 = ORIENTED_EDGE ( 'NONE', *, *, #16184, .T. ) ;
#14775 = DIRECTION ( 'NONE',  ( -0.1566598588826321192, 0.9876526153536342445, 7.798540720466731404E-17 ) ) ;
#14776 = AXIS2_PLACEMENT_3D ( 'NONE', #7718, #17787, #2021 ) ;
#14777 = DIRECTION ( 'NONE',  ( 0.000000000000000000, -1.000000000000000000, -1.914177628664062635E-16 ) ) ;
#14778 = AXIS2_PLACEMENT_3D ( 'NONE', #15061, #766, #18136 ) ;
#14779 = CARTESIAN_POINT ( 'NONE',  ( -48.97054468615517919, -85.72288254658904805, 8.660254037844412167 ) ) ;
#14780 = CONICAL_SURFACE ( 'NONE', #13550, 12.74754878398197633, 0.01745329251994333364 ) ;
#14781 = EDGE_CURVE ( 'NONE', #16710, #10192, #15888, .T. ) ;
#14782 = B_SPLINE_CURVE_WITH_KNOTS ( 'NONE', 3,
 ( #11234, #7008, #4219, #10003, #8601, #8314, #11504, #5764, #15879, #2713, #2883, #8505, #5569, #11316, #17054, #14375 ),
 .UNSPECIFIED., .F., .F.,
 ( 4, 2, 2, 2, 2, 2, 2, 4 ),
 ( 0.000000000000000000, 0.0006035471611761543051, 0.001207094322352308610, 0.001810641483528462698, 0.002414188644704618088, 0.003017735805880773694, 0.003621282967056928866, 0.004828377289409239645 ),
 .UNSPECIFIED. ) ;
#14783 = CARTESIAN_POINT ( 'NONE',  ( -63.82496892663746735, -30.37359899348040315, -4.330127018922181215 ) ) ;
#14784 = DIRECTION ( 'NONE',  ( 3.208277787129350839E-17, 0.000000000000000000, -1.000000000000000000 ) ) ;
#14785 = DIRECTION ( 'NONE',  ( 0.000000000000000000, -1.000000000000000000, 0.000000000000000000 ) ) ;
#14786 = ORIENTED_EDGE ( 'NONE', *, *, #8322, .F. ) ;
#14787 = FILL_AREA_STYLE_COLOUR ( '', #12146 ) ;
#14788 = EDGE_LOOP ( 'NONE', ( #5720, #16924, #9548, #1304 ) ) ;
#14789 = DIRECTION ( 'NONE',  ( -1.000000000000000000, 0.000000000000000000, 0.000000000000000000 ) ) ;
#14790 = AXIS2_PLACEMENT_3D ( 'NONE', #1004, #6576, #12230 ) ;
#14791 = EDGE_CURVE ( 'NONE', #11499, #10533, #7470, .T. ) ;
#14792 = AXIS2_PLACEMENT_3D ( 'NONE', #6059, #16002, #3012 ) ;
#14793 = DIRECTION ( 'NONE',  ( -0.1566598588826321192, 0.9876526153536342445, 7.798540720466730171E-17 ) ) ;
#14794 = EDGE_LOOP ( 'NONE', ( #15408, #9880 ) ) ;
#14795 = ORIENTED_EDGE ( 'NONE', *, *, #13796, .T. ) ;
#14796 = VERTEX_POINT ( 'NONE', #2722 ) ;
#14797 = EDGE_LOOP ( 'NONE', ( #21, #9839 ) ) ;
#14798 = VERTEX_POINT ( 'NONE', #2891 ) ;
#14799 = CARTESIAN_POINT ( 'NONE',  ( -131.1404785418517918, -2.850701963179328668, 9.951701414186818625E-16 ) ) ;
#14800 = FACE_BOUND ( 'NONE', #18690, .T. ) ;
#14801 = EDGE_LOOP ( 'NONE', ( #14192, #12207, #1529, #12598 ) ) ;
#14802 = DIRECTION ( 'NONE',  ( -0.1566598588826321192, 0.9876526153536342445, 7.798540720466731404E-17 ) ) ;
#14803 = CIRCLE ( 'NONE', #906, 1.500000000000000888 ) ;
#14804 = ORIENTED_EDGE ( 'NONE', *, *, #12447, .T. ) ;
#14805 = AXIS2_PLACEMENT_3D ( 'NONE', #8126, #8514, #12480 ) ;
#14806 = AXIS2_PLACEMENT_3D ( 'NONE', #15882, #11775, #4406 ) ;
#14807 = VECTOR ( 'NONE', #5960, 1000.000000000000114 ) ;
#14808 = ORIENTED_EDGE ( 'NONE', *, *, #14373, .F. ) ;
#14809 = ADVANCED_FACE ( 'NONE', ( #8515 ), #7287, .F. ) ;
#14810 = DIRECTION ( 'NONE',  ( -0.1566598588826321192, 0.9876526153536342445, 7.798540720466730171E-17 ) ) ;
#14811 = CARTESIAN_POINT ( 'NONE',  ( 7.819480696678551723, -76.71494066083772623, -12.99038105676658894 ) ) ;
#14813 = EDGE_CURVE ( 'NONE', #6687, #10467, #12850, .T. ) ;
#14812 = FACE_BOUND ( 'NONE', #17333, .T. ) ;
#14814 = VECTOR ( 'NONE', #6662, 1000.000000000000000 ) ;
#14815 = CYLINDRICAL_SURFACE ( 'NONE', #2881, 1.500000000000001554 ) ;
#14816 = CIRCLE ( 'NONE', #1805, 1.500000000000000444 ) ;
#14817 = CARTESIAN_POINT ( 'NONE',  ( -21.81009776393036503, -81.41473642731668292, -4.330127018922185655 ) ) ;
#14818 = ORIENTED_EDGE ( 'NONE', *, *, #18340, .T. ) ;
#14819 = ORIENTED_EDGE ( 'NONE', *, *, #7868, .F. ) ;
#14820 = DIRECTION ( 'NONE',  ( -0.9876526153536336894, -0.1566598588826349503, 0.000000000000000000 ) ) ;
#14821 = CARTESIAN_POINT ( 'NONE',  ( 2.000000000000000000, 0.000000000000000000, -35.00000000000000000 ) ) ;
#14822 = VECTOR ( 'NONE', #16621, 1000.000000000000114 ) ;
#14823 = DIRECTION ( 'NONE',  ( 0.000000000000000000, 0.000000000000000000, 1.000000000000000000 ) ) ;
#14824 = ORIENTED_EDGE ( 'NONE', *, *, #8118, .T. ) ;
#14825 = CIRCLE ( 'NONE', #13590, 1.500000000000000888 ) ;
#14826 = AXIS2_PLACEMENT_3D ( 'NONE', #3339, #17890, #6309 ) ;
#14827 = EDGE_LOOP ( 'NONE', ( #14900, #14863, #17573, #15080 ) ) ;
#14828 = CARTESIAN_POINT ( 'NONE',  ( -81.88695483773778960, -2.621191165925490729, 2.499999999999999112 ) ) ;
#14829 = CARTESIAN_POINT ( 'NONE',  ( -31.72625892764450484, -25.28215357979487266, -17.32050807568878170 ) ) ;
#14830 = VECTOR ( 'NONE', #2051, 1000.000000000000000 ) ;
#14831 = CARTESIAN_POINT ( 'NONE',  ( -68.76323200340563346, -31.15689828789355786, 21.65063509461101887 ) ) ;
#14832 = DIRECTION ( 'NONE',  ( 0.000000000000000000, 0.000000000000000000, 1.000000000000000000 ) ) ;
#14833 = EDGE_CURVE ( 'NONE', #12364, #11399, #3799, .T. ) ;
#14834 = TOROIDAL_SURFACE ( 'NONE', #8775, 15.88900348692940945, 3.000000000000000000 ) ;
#14835 = EDGE_CURVE ( 'NONE', #1680, #14596, #12934, .T. ) ;
#14836 = DIRECTION ( 'NONE',  ( 0.000000000000000000, 0.000000000000000000, 1.000000000000000000 ) ) ;
#14837 = FACE_OUTER_BOUND ( 'NONE', #2181, .T. ) ;
#14838 = AXIS2_PLACEMENT_3D ( 'NONE', #17381, #1710, #16301 ) ;
#14839 = FILL_AREA_STYLE_COLOUR ( '', #822 ) ;
#14840 = CARTESIAN_POINT ( 'NONE',  ( -62.30385499342917655, -87.83779064150456861, -17.32050807568878525 ) ) ;
#14841 = VERTEX_POINT ( 'NONE', #17426 ) ;
#14842 = CARTESIAN_POINT ( 'NONE',  ( 73.09088021254186174, 1.387778780781445676E-14, -25.00000000000000000 ) ) ;
#14843 = ORIENTED_EDGE ( 'NONE', *, *, #8815, .T. ) ;
#14844 = CIRCLE ( 'NONE', #11207, 1.499999999999997335 ) ;
#14845 = CIRCLE ( 'NONE', #6078, 15.88900348692940945 ) ;
#14846 = ORIENTED_EDGE ( 'NONE', *, *, #3117, .T. ) ;
#14847 = VECTOR ( 'NONE', #7449, 1000.000000000000114 ) ;
#14848 = CARTESIAN_POINT ( 'NONE',  ( -56.21322099054477661, -24.10372711620990671, 4.330127018922218518 ) ) ;
#14849 = AXIS2_PLACEMENT_3D ( 'NONE', #235, #8868, #13206 ) ;
#14850 = CARTESIAN_POINT ( 'NONE',  ( -20.82244514857674389, -81.25807656843406335, 8.660254037844412167 ) ) ;
#14851 = CYLINDRICAL_SURFACE ( 'NONE', #12818, 1.500000000000000888 ) ;
#14852 = DIRECTION ( 'NONE',  ( -0.1566598588826321192, 0.9876526153536342445, 7.798540720466730171E-17 ) ) ;
#14853 =( LENGTH_UNIT ( ) NAMED_UNIT ( * ) SI_UNIT ( .MILLI., .METRE. ) );
#14854 = DIRECTION ( 'NONE',  ( 0.000000000000000000, 0.000000000000000000, 1.000000000000000000 ) ) ;
#14855 = LINE ( 'NONE', #13612, #16617 ) ;
#14856 = VECTOR ( 'NONE', #5175, 1000.000000000000000 ) ;
#14857 = DIRECTION ( 'NONE',  ( -0.1566598588826321192, 0.9876526153536342445, 7.798540720466730171E-17 ) ) ;
#14858 = CARTESIAN_POINT ( 'NONE',  ( -56.37793930130741415, -86.89783148820879433, -4.330127018922185655 ) ) ;
#14859 = CIRCLE ( 'NONE', #3958, 1.500000000000000444 ) ;
#14861 = ORIENTED_EDGE ( 'NONE', *, *, #134, .T. ) ;
#14860 = CARTESIAN_POINT ( 'NONE',  ( -47.48906576312472794, -85.48789275826511869, 17.32050807568881368 ) ) ;
#14862 = EDGE_CURVE ( 'NONE', #6605, #14531, #2985, .T. ) ;
#14863 = ORIENTED_EDGE ( 'NONE', *, *, #14894, .F. ) ;
#14864 = EDGE_CURVE ( 'NONE', #1820, #2692, #4229, .T. ) ;
#14865 = CARTESIAN_POINT ( 'NONE',  ( -127.1404785156000941, 9.613695087247908333, 2.500000000000000000 ) ) ;
#14866 = ORIENTED_EDGE ( 'NONE', *, *, #316, .F. ) ;
#14867 = CIRCLE ( 'NONE', #1858, 1.500000000000000444 ) ;
#14868 = ORIENTED_EDGE ( 'NONE', *, *, #15415, .F. ) ;
#14869 = CIRCLE ( 'NONE', #12444, 1.500000000000000444 ) ;
#14870 = DIRECTION ( 'NONE',  ( -0.9876526153536341335, -0.1566598588826327576, 0.000000000000000000 ) ) ;
#14871 = CARTESIAN_POINT ( 'NONE',  ( 2.881217619910392269, -77.49823995525089515, -12.99038105676658539 ) ) ;
#14872 = CIRCLE ( 'NONE', #65, 2.000000000000000000 ) ;
#14873 = FACE_OUTER_BOUND ( 'NONE', #18201, .T. ) ;
#14874 = DIRECTION ( 'NONE',  ( 0.000000000000000000, 0.000000000000000000, 1.000000000000000000 ) ) ;
#14875 = DIRECTION ( 'NONE',  ( -0.1566598588826321192, 0.9876526153536342445, 7.798540720466731404E-17 ) ) ;
#14876 = CIRCLE ( 'NONE', #4889, 2.000000000000000000 ) ;
#14877 = CARTESIAN_POINT ( 'NONE',  ( -349.6046375497077179, 10.42115585936044830, 9.951701414186830458E-16 ) ) ;
#14878 = CARTESIAN_POINT ( 'NONE',  ( -26.74836084069850983, -82.19803572172985184, -4.330127018922185655 ) ) ;
#14879 = CARTESIAN_POINT ( 'NONE',  ( -63.82496892663746735, -30.37359899348039605, 21.65063509461101887 ) ) ;
#14880 = CARTESIAN_POINT ( 'NONE',  ( -77.44775222064782838, -27.47191408218647624, -21.65063509461098334 ) ) ;
#14881 = DIRECTION ( 'NONE',  ( 0.000000000000000000, 0.000000000000000000, 1.000000000000000000 ) ) ;
#14882 = ORIENTED_EDGE ( 'NONE', *, *, #9856, .F. ) ;
#14883 = AXIS2_PLACEMENT_3D ( 'NONE', #10617, #2087, #771 ) ;
#14884 = CARTESIAN_POINT ( 'NONE',  ( -61.15148406731293562, -24.88702641062305432, -21.65063509461097979 ) ) ;
#14885 = ORIENTED_EDGE ( 'NONE', *, *, #5377, .T. ) ;
#14886 = DIRECTION ( 'NONE',  ( -0.1566598588826321192, 0.9876526153536342445, 7.798540720466730171E-17 ) ) ;
#14887 = CARTESIAN_POINT ( 'NONE',  ( -40.61513246582718040, -26.69209230973856251, 4.330127018922217630 ) ) ;
#14888 = AXIS2_PLACEMENT_3D ( 'NONE', #18314, #5572, #12752 ) ;
#14889 = VERTEX_POINT ( 'NONE', #14563 ) ;
#14890 = VERTEX_POINT ( 'NONE', #5935 ) ;
#14891 = ORIENTED_EDGE ( 'NONE', *, *, #2362, .T. ) ;
#14892 = VERTEX_POINT ( 'NONE', #15809 ) ;
#14893 = CYLINDRICAL_SURFACE ( 'NONE', #499, 1.500000000000001554 ) ;
#14894 = EDGE_CURVE ( 'NONE', #1314, #12681, #6584, .T. ) ;
#14895 = EDGE_LOOP ( 'NONE', ( #2609, #11035 ) ) ;
#14896 = ORIENTED_EDGE ( 'NONE', *, *, #738, .T. ) ;
#14897 = FACE_BOUND ( 'NONE', #10430, .T. ) ;
#14898 = VECTOR ( 'NONE', #16420, 1000.000000000000000 ) ;
#14899 = SURFACE_STYLE_USAGE ( .BOTH. , #5018 ) ;
#14900 = ORIENTED_EDGE ( 'NONE', *, *, #3409, .F. ) ;
#14901 = EDGE_CURVE ( 'NONE', #13436, #7195, #17188, .T. ) ;
#14902 = CIRCLE ( 'NONE', #9166, 1.499999999999999556 ) ;
#14903 = ORIENTED_EDGE ( 'NONE', *, *, #15569, .T. ) ;
#14904 = ORIENTED_EDGE ( 'NONE', *, *, #14781, .F. ) ;
#14905 = CARTESIAN_POINT ( 'NONE',  ( 6.338001773648093362, -76.94993044916168401, -21.65063509461098690 ) ) ;
#14906 = CARTESIAN_POINT ( 'NONE',  ( -309.0881213225398483, -2.850701963179328668, 9.951701414186818625E-16 ) ) ;
#14907 = CARTESIAN_POINT ( 'NONE',  ( 0.000000000000000000, 0.000000000000000000, 25.00000000000000000 ) ) ;
#14908 = CARTESIAN_POINT ( 'NONE',  ( -74.31765932953604192, 46.83718354949606066, -2.499999999999997780 ) ) ;
#14909 = DIRECTION ( 'NONE',  ( -0.9876526153536341335, -0.1566598588826327021, 0.000000000000000000 ) ) ;
#14910 = EDGE_LOOP ( 'NONE', ( #393, #10833, #16550, #1412 ) ) ;
#14911 = ORIENTED_EDGE ( 'NONE', *, *, #17341, .F. ) ;
#14912 = DIRECTION ( 'NONE',  ( -0.9876526153536336894, -0.1566598588826349503, 0.000000000000000000 ) ) ;
#14913 = DIRECTION ( 'NONE',  ( 0.000000000000000000, 0.000000000000000000, 1.000000000000000000 ) ) ;
#14914 = FACE_OUTER_BOUND ( 'NONE', #15402, .T. ) ;
#14915 = PLANE ( 'NONE',  #7210 ) ;
#14916 = CIRCLE ( 'NONE', #15835, 1.500000000000000888 ) ;
#14917 = CARTESIAN_POINT ( 'NONE',  ( -70.20507591625822386, -89.09106951256563889, -8.660254037844385522 ) ) ;
#14918 = EDGE_CURVE ( 'NONE', #8286, #7360, #17790, .T. ) ;
#14919 = VERTEX_POINT ( 'NONE', #10735 ) ;
#14920 = CARTESIAN_POINT ( 'NONE',  ( -62.00000000000000000, 0.000000000000000000, -25.00000000000000000 ) ) ;
#14921 = CARTESIAN_POINT ( 'NONE',  ( -72.71384246482016067, -31.78353772342409300, 8.660254037844417496 ) ) ;
#14922 = ORIENTED_EDGE ( 'NONE', *, *, #14833, .F. ) ;
#14923 = EDGE_CURVE ( 'NONE', #11443, #1825, #1145, .T. ) ;
#14924 = DIRECTION ( 'NONE',  ( -0.1566598588826321747, 0.9876526153536343555, 0.000000000000000000 ) ) ;
#14925 = DIRECTION ( 'NONE',  ( -0.1566598588826321747, 0.9876526153536343555, 0.000000000000000000 ) ) ;
#14926 = CARTESIAN_POINT ( 'NONE',  ( -23.29157668696081629, -81.64972621564064070, -12.99038105676658539 ) ) ;
#14927 = AXIS2_PLACEMENT_3D ( 'NONE', #940, #18403, #2241 ) ;
#14928 = CARTESIAN_POINT ( 'NONE',  ( -19.17624791478365864, -18.22898240811121440, -8.660254037844380193 ) ) ;
#14929 = CARTESIAN_POINT ( 'NONE',  ( 55.85952145814821534, 6.938893903907228378E-15, -2.500000000000000000 ) ) ;
#14930 = ORIENTED_EDGE ( 'NONE', *, *, #14306, .F. ) ;
#14931 = ORIENTED_EDGE ( 'NONE', *, *, #5698, .F. ) ;
#14932 = FACE_OUTER_BOUND ( 'NONE', #7073, .T. ) ;
#14933 = ORIENTED_EDGE ( 'NONE', *, *, #9005, .F. ) ;
#14934 = VERTEX_POINT ( 'NONE', #16461 ) ;
#14935 = DIRECTION ( 'NONE',  ( 0.000000000000000000, 0.000000000000000000, 1.000000000000000000 ) ) ;
#14936 = ORIENTED_EDGE ( 'NONE', *, *, #2829, .T. ) ;
#14937 = ADVANCED_FACE ( 'NONE', ( #6224 ), #10663, .F. ) ;
#14938 = VECTOR ( 'NONE', #5072, 1000.000000000000000 ) ;
#14939 = EDGE_CURVE ( 'NONE', #7705, #9461, #3518, .T. ) ;
#14940 = DIRECTION ( 'NONE',  ( -0.1566598588826321192, 0.9876526153536342445, 7.798540720466730171E-17 ) ) ;
#14941 = ADVANCED_FACE ( 'NONE', ( #17714 ), #9160, .F. ) ;
#14942 = CYLINDRICAL_SURFACE ( 'NONE', #13641, 1.500000000000001554 ) ;
#14943 = EDGE_CURVE ( 'NONE', #2756, #1785, #8685, .T. ) ;
#14944 = DIRECTION ( 'NONE',  ( -0.000000000000000000, -0.000000000000000000, -1.000000000000000000 ) ) ;
#14945 = DIRECTION ( 'NONE',  ( -0.9876526153536341335, -0.1566598588826327021, 0.000000000000000000 ) ) ;
#14946 = ADVANCED_FACE ( 'NONE', ( #17907 ), #13587, .F. ) ;
#14947 = LINE ( 'NONE', #1965, #18494 ) ;
#14948 = CYLINDRICAL_SURFACE ( 'NONE', #9564, 1.500000000000001554 ) ;
#14949 = VERTEX_POINT ( 'NONE', #2036 ) ;
#14950 = DIRECTION ( 'NONE',  ( -0.1566598588826321192, 0.9876526153536342445, 7.798540720466731404E-17 ) ) ;
#14951 = ORIENTED_EDGE ( 'NONE', *, *, #13537, .F. ) ;
#14952 = CARTESIAN_POINT ( 'NONE',  ( 11.77009115809307715, -76.08830122530719109, -8.660254037844389075 ) ) ;
#14954 = VERTEX_POINT ( 'NONE', #13315 ) ;
#14953 = DIRECTION ( 'NONE',  ( 0.000000000000000000, 0.000000000000000000, 1.000000000000000000 ) ) ;
#14955 = LINE ( 'NONE', #18027, #1727 ) ;
#14956 = ORIENTED_EDGE ( 'NONE', *, *, #8837, .F. ) ;
#14958 = ORIENTED_EDGE ( 'NONE', *, *, #16094, .F. ) ;
#14957 = EDGE_CURVE ( 'NONE', #897, #18049, #8984, .T. ) ;
#14959 = CARTESIAN_POINT ( 'NONE',  ( 2.881217619910392269, -77.49823995525089515, -4.330127018922189208 ) ) ;
#14960 = ADVANCED_FACE ( 'NONE', ( #436 ), #4781, .F. ) ;
#14961 = EDGE_LOOP ( 'NONE', ( #18657, #11199, #14502, #17432 ) ) ;
#14962 = CARTESIAN_POINT ( 'NONE',  ( -35.63723437888118184, -83.60797445167352748, 1.424741226644455312E-14 ) ) ;
#14963 = VERTEX_POINT ( 'NONE', #346 ) ;
#14964 = MANIFOLD_SOLID_BREP ( 'Fillet4', #3268 ) ;
#14965 = DIRECTION ( 'NONE',  ( -0.9876526153536341335, -0.1566598588826327021, 0.000000000000000000 ) ) ;
#14966 = DIRECTION ( 'NONE',  ( 0.000000000000000000, 0.000000000000000000, 1.000000000000000000 ) ) ;
#14967 = CARTESIAN_POINT ( 'NONE',  ( -170.5980861165185445, 32.53234180668174247, -5.500000000000001776 ) ) ;
#14968 = EDGE_CURVE ( 'NONE', #18371, #18389, #7485, .T. ) ;
#14969 = PRODUCT_DEFINITION_CONTEXT ( 'detailed design', #13300, 'design' ) ;
#14970 = DIRECTION ( 'NONE',  ( -0.1566598588826321192, 0.9876526153536342445, 7.798540720466730171E-17 ) ) ;
#14971 = DIRECTION ( 'NONE',  ( 0.000000000000000000, 0.000000000000000000, 1.000000000000000000 ) ) ;
#14972 = AXIS2_PLACEMENT_3D ( 'NONE', #1995, #17957, #10701 ) ;
#14973 = CARTESIAN_POINT ( 'NONE',  ( -26.58364252993588650, -19.40393134973095002, -21.65063509461097979 ) ) ;
#14974 = CYLINDRICAL_SURFACE ( 'NONE', #3545, 1.500000000000001554 ) ;
#14975 = ORIENTED_EDGE ( 'NONE', *, *, #18100, .T. ) ;
#14976 = DIRECTION ( 'NONE',  ( -0.1566598588826321192, 0.9876526153536342445, 7.798540720466731404E-17 ) ) ;
#14977 = ORIENTED_EDGE ( 'NONE', *, *, #16208, .F. ) ;
#14978 = CARTESIAN_POINT ( 'NONE',  ( -62.30385499342917655, -87.83779064150456861, -8.660254037844385522 ) ) ;
#14979 = ORIENTED_EDGE ( 'NONE', *, *, #4950, .F. ) ;
#14980 = CARTESIAN_POINT ( 'NONE',  ( -59.83472345504510770, -87.44614099429800547, 12.99038105676661203 ) ) ;
#14981 = PRODUCT_DEFINITION_SHAPE ( 'NONE', 'NONE',  #18795 ) ;
#14982 = ORIENTED_EDGE ( 'NONE', *, *, #16168, .T. ) ;
#14983 = DIRECTION ( 'NONE',  ( -0.000000000000000000, -0.000000000000000000, 1.000000000000000000 ) ) ;
#14984 = ORIENTED_EDGE ( 'NONE', *, *, #2607, .T. ) ;
#14985 = VERTEX_POINT ( 'NONE', #2512 ) ;
#14986 = DIRECTION ( 'NONE',  ( -0.000000000000000000, -0.000000000000000000, -1.000000000000000000 ) ) ;
#14987 = ORIENTED_EDGE ( 'NONE', *, *, #2555, .F. ) ;
#14988 = AXIS2_PLACEMENT_3D ( 'NONE', #9332, #15118, #2137 ) ;
#14989 = FACE_BOUND ( 'NONE', #17776, .T. ) ;
#14990 = CARTESIAN_POINT ( 'NONE',  ( -21.81009776393036503, -81.41473642731668292, -4.330127018922185655 ) ) ;
#14991 = ORIENTED_EDGE ( 'NONE', *, *, #14460, .T. ) ;
#14992 = EDGE_CURVE ( 'NONE', #3473, #13798, #6595, .T. ) ;
#14993 = EDGE_CURVE ( 'NONE', #10341, #14647, #3806, .T. ) ;
#14994 = ORIENTED_EDGE ( 'NONE', *, *, #4909, .T. ) ;
#14995 = DIRECTION ( 'NONE',  ( 0.000000000000000000, 0.000000000000000000, 1.000000000000000000 ) ) ;
#14996 = EDGE_CURVE ( 'NONE', #5613, #13071, #15949, .T. ) ;
#14997 = CARTESIAN_POINT ( 'NONE',  ( -25.26688191766805858, -81.96304593340589406, 4.330127018922213189 ) ) ;
#14998 = VECTOR ( 'NONE', #3605, 1000.000000000000000 ) ;
#14999 = CARTESIAN_POINT ( 'NONE',  ( -65.30644784966791860, -30.60858878180435028, 21.65063509461101887 ) ) ;
#15000 = DIRECTION ( 'NONE',  ( -0.1566598588826321192, 0.9876526153536342445, 7.798540720466730171E-17 ) ) ;
#15001 = CARTESIAN_POINT ( 'NONE',  ( -69.25705831108246002, -31.23522821733487476, 8.660254037844417496 ) ) ;
#15002 = CARTESIAN_POINT ( 'NONE',  ( -41.56315007100297265, -84.54793360496931598, -12.99038105676658539 ) ) ;
#15003 = EDGE_LOOP ( 'NONE', ( #10383, #3196, #13016, #103 ) ) ;
#15004 = VERTEX_POINT ( 'NONE', #5359 ) ;
#15005 = CARTESIAN_POINT ( 'NONE',  ( -79.05438463828195950, 1.499069270643396345, 3.389939594122236333 ) ) ;
#15006 = CARTESIAN_POINT ( 'NONE',  ( -174.8673125818257006, 55.13264502119463373, -5.500000000000001776 ) ) ;
#15007 = CARTESIAN_POINT ( 'NONE',  ( -65.37641414873199608, -43.03264333350146131, -20.00000000000000000 ) ) ;
#15008 = AXIS2_PLACEMENT_3D ( 'NONE', #997, #6768, #3878 ) ;
#15009 = ORIENTED_EDGE ( 'NONE', *, *, #15944, .T. ) ;
#15010 = DIRECTION ( 'NONE',  ( -0.1566598588826321192, 0.9876526153536342445, 7.798540720466730171E-17 ) ) ;
#15011 = AXIS2_PLACEMENT_3D ( 'NONE', #2554, #16703, #18249 ) ;
#15012 = FACE_BOUND ( 'NONE', #14291, .T. ) ;
#15013 = DIRECTION ( 'NONE',  ( -0.9876526153536341335, -0.1566598588826327021, 0.000000000000000000 ) ) ;
#15014 = CARTESIAN_POINT ( 'NONE',  ( -57.20087360589840131, -24.26038697509254405, 8.660254037844417496 ) ) ;
#15015 = ORIENTED_EDGE ( 'NONE', *, *, #16898, .T. ) ;
#15016 = EDGE_CURVE ( 'NONE', #2581, #1938, #15394, .T. ) ;
#15017 = FACE_BOUND ( 'NONE', #3812, .T. ) ;
#15018 = CARTESIAN_POINT ( 'NONE',  ( -25.10216360690543524, -19.16894156140701710, 12.99038105676661736 ) ) ;
#15019 = CARTESIAN_POINT ( 'NONE',  ( 0.000000000000000000, 0.000000000000000000, -20.00000000000000355 ) ) ;
#15020 = ORIENTED_EDGE ( 'NONE', *, *, #8296, .T. ) ;
#15021 = DIRECTION ( 'NONE',  ( -0.9876526153536341335, -0.1566598588826327021, 0.000000000000000000 ) ) ;
#15022 = AXIS2_PLACEMENT_3D ( 'NONE', #7850, #6446, #4708 ) ;
#15023 = VERTEX_POINT ( 'NONE', #2132 ) ;
#15024 = EDGE_CURVE ( 'NONE', #1839, #12162, #2634, .T. ) ;
#15025 = VERTEX_POINT ( 'NONE', #6887 ) ;
#15026 = FACE_OUTER_BOUND ( 'NONE', #16246, .T. ) ;
#15027 = VERTEX_POINT ( 'NONE', #8202 ) ;
#15028 = AXIS2_PLACEMENT_3D ( 'NONE', #11993, #8990, #7762 ) ;
#15029 = DIRECTION ( 'NONE',  ( -0.9876526153536336894, -0.1566598588826349503, 0.000000000000000000 ) ) ;
#15030 = DIRECTION ( 'NONE',  ( -0.1566598588826321192, 0.9876526153536342445, 7.798540720466730171E-17 ) ) ;
#15031 = DIRECTION ( 'NONE',  ( -0.9876526153536336894, -0.1566598588826350336, 0.000000000000000000 ) ) ;
#15032 = VECTOR ( 'NONE', #5052, 1000.000000000000000 ) ;
#15033 = ADVANCED_FACE ( 'NONE', ( #919 ), #16750, .F. ) ;
#15034 = EDGE_LOOP ( 'NONE', ( #3496, #10126, #2231, #14808, #11475, #6306, #13434, #18614, #7404, #6589 ) ) ;
#15035 = DIRECTION ( 'NONE',  ( -0.1566598588826321192, 0.9876526153536342445, 7.798540720466730171E-17 ) ) ;
#15036 =( NAMED_UNIT ( * ) PLANE_ANGLE_UNIT ( ) SI_UNIT ( $, .RADIAN. ) );
#15037 = CARTESIAN_POINT ( 'NONE',  ( -11.93357161039406300, -79.84813783849035929, -21.65063509461098690 ) ) ;
#15038 = FACE_OUTER_BOUND ( 'NONE', #2522, .T. ) ;
#15039 = VECTOR ( 'NONE', #17723, 1000.000000000000114 ) ;
#15040 = AXIS2_PLACEMENT_3D ( 'NONE', #5578, #11325, #15698 ) ;
#15041 = EDGE_CURVE ( 'NONE', #4072, #9210, #16938, .T. ) ;
#15042 = DIRECTION ( 'NONE',  ( -0.1566598588826321192, 0.9876526153536342445, 7.798540720466730171E-17 ) ) ;
#15043 = ORIENTED_EDGE ( 'NONE', *, *, #8805, .F. ) ;
#15044 = DIRECTION ( 'NONE',  ( 1.000000000000000000, 0.000000000000000000, 0.000000000000000000 ) ) ;
#15045 = EDGE_CURVE ( 'NONE', #6246, #13520, #13503, .T. ) ;
#15047 = ORIENTED_EDGE ( 'NONE', *, *, #7031, .T. ) ;
#15046 = CARTESIAN_POINT ( 'NONE',  ( -89.99999999999998579, -35.00000000000001421, 35.00000000000000000 ) ) ;
#15048 = EDGE_CURVE ( 'NONE', #9221, #3679, #5964, .T. ) ;
#15049 = DIRECTION ( 'NONE',  ( 0.000000000000000000, 0.000000000000000000, 1.000000000000000000 ) ) ;
#15050 = VERTEX_POINT ( 'NONE', #2312 ) ;
#15051 = AXIS2_PLACEMENT_3D ( 'NONE', #8594, #15790, #18765 ) ;
#15052 = ORIENTED_EDGE ( 'NONE', *, *, #7659, .T. ) ;
#15053 = DIRECTION ( 'NONE',  ( -0.9876526153536341335, -0.1566598588826327021, 0.000000000000000000 ) ) ;
#15054 = ORIENTED_EDGE ( 'NONE', *, *, #2436, .F. ) ;
#15055 = CIRCLE ( 'NONE', #14748, 1.500000000000000444 ) ;
#15056 = CARTESIAN_POINT ( 'NONE',  ( -10.28737437660097775, -16.81904367816753165, 21.65063509461101177 ) ) ;
#15057 = ORIENTED_EDGE ( 'NONE', *, *, #13362, .T. ) ;
#15058 = DIRECTION ( 'NONE',  ( -0.9876526153536341335, -0.1566598588826327021, 0.000000000000000000 ) ) ;
#15059 = CARTESIAN_POINT ( 'NONE',  ( -129.1404785418517918, -2.850701963179326892, 13.78215425775057845 ) ) ;
#15060 = EDGE_CURVE ( 'NONE', #16292, #16602, #9730, .T. ) ;
#15061 = CARTESIAN_POINT ( 'NONE',  ( -77.72973689007648090, 30.96463005215034059, -35.00000000000000000 ) ) ;
#15062 = PLANE ( 'NONE',  #16050 ) ;
#15063 = FACE_OUTER_BOUND ( 'NONE', #1135, .T. ) ;
#15064 = EDGE_CURVE ( 'NONE', #10341, #1641, #7781, .T. ) ;
#15065 = ORIENTED_EDGE ( 'NONE', *, *, #2335, .T. ) ;
#15066 = AXIS2_PLACEMENT_3D ( 'NONE', #7122, #12782, #2908 ) ;
#15067 = EDGE_CURVE ( 'NONE', #4379, #14, #8095, .T. ) ;
#15068 = CYLINDRICAL_SURFACE ( 'NONE', #12535, 171.3327290851023292 ) ;
#15069 = CARTESIAN_POINT ( 'NONE',  ( -84.23462711737164454, 33.01666666666666572, 35.00000000000000000 ) ) ;
#15070 = CIRCLE ( 'NONE', #7817, 1.500000000000000888 ) ;
#15071 = ORIENTED_EDGE ( 'NONE', *, *, #12361, .T. ) ;
#15072 = VERTEX_POINT ( 'NONE', #11017 ) ;
#15073 = EDGE_LOOP ( 'NONE', ( #6475, #3757, #15262, #10601 ) ) ;
#15074 = CYLINDRICAL_SURFACE ( 'NONE', #5648, 1.500000000000001554 ) ;
#15075 = AXIS2_PLACEMENT_3D ( 'NONE', #13531, #581, #6371 ) ;
#15076 = FACE_BOUND ( 'NONE', #13095, .T. ) ;
#15077 = PRESENTATION_LAYER_ASSIGNMENT (  '', '', ( #2067 ) ) ;
#15078 = DIRECTION ( 'NONE',  ( 0.000000000000000000, 0.000000000000000000, 1.000000000000000000 ) ) ;
#15079 = DIRECTION ( 'NONE',  ( -0.1566598588826321192, 0.9876526153536342445, 7.798540720466730171E-17 ) ) ;
#15080 = ORIENTED_EDGE ( 'NONE', *, *, #14761, .T. ) ;
#15081 = CIRCLE ( 'NONE', #12044, 1.500000000000000888 ) ;
#15082 = AXIS2_PLACEMENT_3D ( 'NONE', #15619, #8255, #2553 ) ;
#15083 = VERTEX_POINT ( 'NONE', #14061 ) ;
#15084 = DIRECTION ( 'NONE',  ( -0.1566598588826321192, 0.9876526153536342445, 7.798540720466730171E-17 ) ) ;
#15085 = EDGE_LOOP ( 'NONE', ( #8044, #1573 ) ) ;
#15086 = DIRECTION ( 'NONE',  ( -0.1566598588826321192, 0.9876526153536342445, 7.798540720466730171E-17 ) ) ;
#15087 = DIRECTION ( 'NONE',  ( -0.1566598588826321192, 0.9876526153536342445, 7.798540720466730171E-17 ) ) ;
#15088 = CARTESIAN_POINT ( 'NONE',  ( -306.0881213225399051, -2.850701963179328668, 9.951701414186818625E-16 ) ) ;
#15089 = ORIENTED_EDGE ( 'NONE', *, *, #2341, .F. ) ;
#15090 = ORIENTED_EDGE ( 'NONE', *, *, #10140, .T. ) ;
#15091 = CARTESIAN_POINT ( 'NONE',  ( -16.70711637639958269, -17.83733276090463704, 4.330127018922218518 ) ) ;
#15092 = FACE_OUTER_BOUND ( 'NONE', #10404, .T. ) ;
#15093 = LINE ( 'NONE', #7905, #15357 ) ;
#15094 = EDGE_CURVE ( 'NONE', #10171, #7400, #12599, .T. ) ;
#15095 = CARTESIAN_POINT ( 'NONE',  ( -19.38060123572413218, -23.32390534376198232, 4.330127018922217630 ) ) ;
#15096 = CIRCLE ( 'NONE', #14201, 1.499999999999999556 ) ;
#15097 = ORIENTED_EDGE ( 'NONE', *, *, #6732, .T. ) ;
#15098 = EDGE_CURVE ( 'NONE', #8327, #5727, #6893, .T. ) ;
#15099 = AXIS2_PLACEMENT_3D ( 'NONE', #5027, #707, #9597 ) ;
#15100 = ORIENTED_EDGE ( 'NONE', *, *, #2582, .T. ) ;
#15101 = CARTESIAN_POINT ( 'NONE',  ( -32.50955822205765600, -20.34389050302674207, -17.32050807568878170 ) ) ;
#15102 = CARTESIAN_POINT ( 'NONE',  ( -52.96079015774756726, -28.65034054577146705, -17.32050807568878170 ) ) ;
#15103 = CIRCLE ( 'NONE', #3290, 1.500000000000000888 ) ;
#15104 = CARTESIAN_POINT ( 'NONE',  ( -173.5975526607244035, 56.27156339024950427, -2.918139657044712454 ) ) ;
#15105 = EDGE_CURVE ( 'NONE', #12855, #3591, #12248, .T. ) ;
#15106 = AXIS2_PLACEMENT_3D ( 'NONE', #2885, #18775, #4501 ) ;
#15107 = CIRCLE ( 'NONE', #6657, 1.500000000000001332 ) ;
#15108 = DIRECTION ( 'NONE',  ( -0.1566598588826321192, 0.9876526153536342445, 7.798540720466730171E-17 ) ) ;
#15109 = FACE_OUTER_BOUND ( 'NONE', #3415, .T. ) ;
#15110 = DIRECTION ( 'NONE',  ( -0.1566598588826321192, 0.9876526153536342445, 7.798540720466730171E-17 ) ) ;
#15111 = CARTESIAN_POINT ( 'NONE',  ( 0.000000000000000000, 0.000000000000000000, 0.000000000000000000 ) ) ;
#15112 = CIRCLE ( 'NONE', #15710, 1.500000000000000888 ) ;
#15113 = CARTESIAN_POINT ( 'NONE',  ( -79.13358446461874962, -32.80182680616118773, 1.869203119972154228E-14 ) ) ;
#15115 = DIRECTION ( 'NONE',  ( -1.000000000000000000, -3.469446951953611033E-15, 0.000000000000000000 ) ) ;
#15114 = CIRCLE ( 'NONE', #18506, 1.500000000000000888 ) ;
#15116 = ORIENTED_EDGE ( 'NONE', *, *, #1826, .T. ) ;
#15117 = LINE ( 'NONE', #16113, #559 ) ;
#15118 = DIRECTION ( 'NONE',  ( -0.1566598588826321747, 0.9876526153536343555, 0.000000000000000000 ) ) ;
#15119 = AXIS2_PLACEMENT_3D ( 'NONE', #16059, #1568, #7260 ) ;
#15120 = ORIENTED_EDGE ( 'NONE', *, *, #9378, .T. ) ;
#15121 = ORIENTED_EDGE ( 'NONE', *, *, #15384, .F. ) ;
#15122 = DIRECTION ( 'NONE',  ( -0.1566598588826321192, 0.9876526153536342445, 7.798540720466731404E-17 ) ) ;
#15123 = VECTOR ( 'NONE', #9063, 1000.000000000000000 ) ;
#15124 = AXIS2_PLACEMENT_3D ( 'NONE', #16037, #8736, #11374 ) ;
#15125 = ORIENTED_EDGE ( 'NONE', *, *, #13666, .F. ) ;
#15126 = MANIFOLD_SOLID_BREP ( 'Boss-Extrude1', #12660 ) ;
#15127 = VERTEX_POINT ( 'NONE', #2871 ) ;
#15128 = ORIENTED_EDGE ( 'NONE', *, *, #6644, .F. ) ;
#15129 = AXIS2_PLACEMENT_3D ( 'NONE', #7594, #10415, #17382 ) ;
#15130 = ADVANCED_FACE ( 'NONE', ( #11486, #14358 ), #3629, .F. ) ;
#15131 = AXIS2_PLACEMENT_3D ( 'NONE', #14811, #4663, #17695 ) ;
#15132 = CARTESIAN_POINT ( 'NONE',  ( -20.86208015875457988, -23.55889513208593655, -12.99038105676658006 ) ) ;
#15133 = AXIS2_PLACEMENT_3D ( 'NONE', #5239, #16914, #15473 ) ;
#15134 = DIRECTION ( 'NONE',  ( 0.000000000000000000, 0.000000000000000000, 1.000000000000000000 ) ) ;
#15135 = DIRECTION ( 'NONE',  ( -0.9876526153536341335, -0.1566598588826327576, 0.000000000000000000 ) ) ;
#15136 = AXIS2_PLACEMENT_3D ( 'NONE', #7956, #18034, #760 ) ;
#15137 = CARTESIAN_POINT ( 'NONE',  ( -12.75650591498505371, -17.21069332537411256, 17.32050807568881012 ) ) ;
#15138 = EDGE_CURVE ( 'NONE', #16734, #1864, #17323, .T. ) ;
#15139 = CARTESIAN_POINT ( 'NONE',  ( -18.35331361019266794, -80.86642692122748599, 12.99038105676661203 ) ) ;
#15140 = DIRECTION ( 'NONE',  ( -0.9998476951563911586, 0.000000000000000000, -0.01745240643728354635 ) ) ;
#15141 = AXIS2_PLACEMENT_3D ( 'NONE', #1239, #12567, #9557 ) ;
#15142 = CARTESIAN_POINT ( 'NONE',  ( 3.231158466157551423, 19.73726462726227737, -30.00000000000000000 ) ) ;
#15143 = ORIENTED_EDGE ( 'NONE', *, *, #1852, .T. ) ;
#15144 = CARTESIAN_POINT ( 'NONE',  ( -76.88766983611584749, -2.536636612185957595, -7.500000000000000000 ) ) ;
#15145 = AXIS2_PLACEMENT_3D ( 'NONE', #11373, #15559, #12892 ) ;
#15147 = ORIENTED_EDGE ( 'NONE', *, *, #1045, .F. ) ;
#15146 = CARTESIAN_POINT ( 'NONE',  ( -76.95392591297100182, -27.39358415274516645, -17.32050807568878170 ) ) ;
#15148 = ORIENTED_EDGE ( 'NONE', *, *, #18484, .F. ) ;
#15149 = CIRCLE ( 'NONE', #3626, 1.500000000000000888 ) ;
#15150 = CARTESIAN_POINT ( 'NONE',  ( -0.1213752363283457369, -20.26903809555066616, -8.660254037844383745 ) ) ;
#15151 = CIRCLE ( 'NONE', #14838, 1.500000000000001332 ) ;
#15152 = EDGE_CURVE ( 'NONE', #14323, #10331, #8699, .T. ) ;
#15153 = ORIENTED_EDGE ( 'NONE', *, *, #12823, .T. ) ;
#15154 = CIRCLE ( 'NONE', #17612, 1.500000000000000000 ) ;
#15155 = EDGE_CURVE ( 'NONE', #11172, #495, #10497, .T. ) ;
#15156 = CARTESIAN_POINT ( 'NONE',  ( -60.32854976272193426, -87.52447092373931525, -17.32050807568878525 ) ) ;
#15157 = VECTOR ( 'NONE', #67, 1000.000000000000000 ) ;
#15158 = DIRECTION ( 'NONE',  ( -0.9876526153536336894, -0.1566598588826350336, 0.000000000000000000 ) ) ;
#15159 = AXIS2_PLACEMENT_3D ( 'NONE', #10667, #4883, #11879 ) ;
#15160 = ORIENTED_EDGE ( 'NONE', *, *, #6145, .F. ) ;
#15161 = DIRECTION ( 'NONE',  ( -0.1566598588826321192, 0.9876526153536342445, 7.798540720466730171E-17 ) ) ;
#15162 = EDGE_CURVE ( 'NONE', #16506, #5655, #16260, .T. ) ;
#15163 = CARTESIAN_POINT ( 'NONE',  ( -79.91688375903190433, -27.86356372939306780, 8.660254037844417496 ) ) ;
#15164 = CARTESIAN_POINT ( 'NONE',  ( -58.84707083969148300, -87.28948113541537168, 8.660254037844412167 ) ) ;
#15165 = CARTESIAN_POINT ( 'NONE',  ( -85.86167379012967160, 34.32252072304513746, -30.00000000000000000 ) ) ;
#15166 = VERTEX_POINT ( 'NONE', #8668 ) ;
#15167 = CIRCLE ( 'NONE', #5815, 1.500000000000000888 ) ;
#15168 = CYLINDRICAL_SURFACE ( 'NONE', #17038, 1.500000000000001554 ) ;
#15169 = CARTESIAN_POINT ( 'NONE',  ( -72.01566283620284992, -26.61028485833201529, 1.926565525561697761E-14 ) ) ;
#15170 = VECTOR ( 'NONE', #4792, 1000.000000000000000 ) ;
#15171 = FACE_OUTER_BOUND ( 'NONE', #6448, .T. ) ;
#15172 = ORIENTED_EDGE ( 'NONE', *, *, #3201, .F. ) ;
#15173 = EDGE_LOOP ( 'NONE', ( #11944, #1766 ) ) ;
#15174 = ORIENTED_EDGE ( 'NONE', *, *, #5337, .T. ) ;
#15175 = ORIENTED_EDGE ( 'NONE', *, *, #15094, .T. ) ;
#15176 = DIRECTION ( 'NONE',  ( -0.000000000000000000, -0.000000000000000000, -1.000000000000000000 ) ) ;
#15177 = EDGE_CURVE ( 'NONE', #2115, #15396, #2331, .T. ) ;
#15178 = AXIS2_PLACEMENT_3D ( 'NONE', #15445, #11159, #8253 ) ;
#15179 = ORIENTED_EDGE ( 'NONE', *, *, #1297, .T. ) ;
#15180 = FACE_BOUND ( 'NONE', #9399, .T. ) ;
#15181 = EDGE_CURVE ( 'NONE', #1617, #6871, #11988, .T. ) ;
#15182 = EDGE_CURVE ( 'NONE', #11831, #9589, #15351, .T. ) ;
#15183 = VERTEX_POINT ( 'NONE', #11396 ) ;
#15184 = EDGE_CURVE ( 'NONE', #17699, #9820, #11101, .T. ) ;
#15185 = DIRECTION ( 'NONE',  ( -0.1566598588826321747, 0.9876526153536343555, 0.000000000000000000 ) ) ;
#15186 = ORIENTED_EDGE ( 'NONE', *, *, #17341, .T. ) ;
#15187 = AXIS2_PLACEMENT_3D ( 'NONE', #7710, #13462, #504 ) ;
#15188 = CIRCLE ( 'NONE', #17649, 1.500000000000000888 ) ;
#15189 = DIRECTION ( 'NONE',  ( -0.1615579233078772992, -0.9868632313631134911, 0.000000000000000000 ) ) ;
#15190 = DIRECTION ( 'NONE',  ( -0.1566598588826321192, 0.9876526153536342445, 7.798540720466731404E-17 ) ) ;
#15191 = CARTESIAN_POINT ( 'NONE',  ( -89.99999999999998579, -35.00000000000001421, 100.5765140304660861 ) ) ;
#15192 = AXIS2_PLACEMENT_3D ( 'NONE', #3474, #7407, #10409 ) ;
#15193 = CARTESIAN_POINT ( 'NONE',  ( -16.87183468716221313, -80.63143713290352821, -12.99038105676658539 ) ) ;
#15194 = ORIENTED_EDGE ( 'NONE', *, *, #14996, .T. ) ;
#15195 = ORIENTED_EDGE ( 'NONE', *, *, #11042, .T. ) ;
#15196 = DIRECTION ( 'NONE',  ( -0.1566598588826321192, 0.9876526153536342445, 7.798540720466730171E-17 ) ) ;
#15197 = CYLINDRICAL_SURFACE ( 'NONE', #6596, 1.500000000000001554 ) ;
#15198 = AXIS2_PLACEMENT_3D ( 'NONE', #10422, #11834, #4370 ) ;
#15199 = EDGE_LOOP ( 'NONE', ( #15270, #13545 ) ) ;
#15200 = VERTEX_POINT ( 'NONE', #17219 ) ;
#15201 = CARTESIAN_POINT ( 'NONE',  ( -89.99999999999998579, -35.00000000000001421, -35.00000000000000000 ) ) ;
#15202 = DIRECTION ( 'NONE',  ( -0.1566598588826321747, 0.9876526153536343555, 0.000000000000000000 ) ) ;
#15203 = VECTOR ( 'NONE', #6103, 1000.000000000000114 ) ;
#15204 = DIRECTION ( 'NONE',  ( -1.000000000000000000, 0.000000000000000000, 0.000000000000000000 ) ) ;
#15205 = B_SPLINE_CURVE_WITH_KNOTS ( 'NONE', 3,
 ( #18695, #5667, #16707, #13820, #7289, #16085 ),
 .UNSPECIFIED., .F., .F.,
 ( 4, 2, 4 ),
 ( 0.000000000000000000, 0.001759783889192315272, 0.003519567778384630544 ),
 .UNSPECIFIED. ) ;
#15206 = DIRECTION ( 'NONE',  ( -0.9876526153536344665, -0.1566598588826304539, 0.000000000000000000 ) ) ;
#15207 = CARTESIAN_POINT ( 'NONE',  ( 0.000000000000000000, 0.000000000000000000, -35.00000000000000000 ) ) ;
#15208 = ADVANCED_FACE ( 'NONE', ( #15576 ), #5740, .F. ) ;
#15209 = ADVANCED_FACE ( 'NONE', ( #14446 ), #15958, .F. ) ;
#15210 = DIRECTION ( 'NONE',  ( -0.9876526153536341335, -0.1566598588826327021, 0.000000000000000000 ) ) ;
#15211 = FILL_AREA_STYLE ('',( #9434 ) ) ;
#15212 = DIRECTION ( 'NONE',  ( -0.1566598588826321192, 0.9876526153536342445, 7.798540720466730171E-17 ) ) ;
#15213 = EDGE_LOOP ( 'NONE', ( #10741, #18234, #2825, #1077 ) ) ;
#15214 = ORIENTED_EDGE ( 'NONE', *, *, #9618, .F. ) ;
#15215 = CIRCLE ( 'NONE', #11866, 1.500000000000000888 ) ;
#15216 = DIRECTION ( 'NONE',  ( -0.1566598588826321747, 0.9876526153536343555, 0.000000000000000000 ) ) ;
#15217 = VERTEX_POINT ( 'NONE', #14269 ) ;
#15218 = ORIENTED_EDGE ( 'NONE', *, *, #9952, .T. ) ;
#15219 = FACE_OUTER_BOUND ( 'NONE', #16401, .T. ) ;
#15220 = LINE ( 'NONE', #2239, #3639 ) ;
#15221 = AXIS2_PLACEMENT_3D ( 'NONE', #13252, #6460, #4913 ) ;
#15222 = ORIENTED_EDGE ( 'NONE', *, *, #11966, .T. ) ;
#15223 = CARTESIAN_POINT ( 'NONE',  ( -47.98289207080154739, -85.56622268770644268, 21.65063509461101532 ) ) ;
#15224 = ORIENTED_EDGE ( 'NONE', *, *, #16102, .T. ) ;
#15225 = CARTESIAN_POINT ( 'NONE',  ( 0.000000000000000000, 0.000000000000000000, -20.00000000000000355 ) ) ;
#15226 = EDGE_CURVE ( 'NONE', #1436, #11647, #5680, .T. ) ;
#15227 = ADVANCED_FACE ( 'NONE', ( #6990 ), #12730, .F. ) ;
#15228 = CYLINDRICAL_SURFACE ( 'NONE', #7846, 1.500000000000001554 ) ;
#15229 = DIRECTION ( 'NONE',  ( -0.9876526153536336894, -0.1566598588826349503, 0.000000000000000000 ) ) ;
#15230 = CARTESIAN_POINT ( 'NONE',  ( -25.76070822534488869, -82.04137586284720385, 1.424741226644455312E-14 ) ) ;
#15231 = DIRECTION ( 'NONE',  ( -0.1566598588826321192, 0.9876526153536342445, 7.798540720466730171E-17 ) ) ;
#15232 = EDGE_CURVE ( 'NONE', #10493, #592, #10575, .T. ) ;
#15234 = ORIENTED_EDGE ( 'NONE', *, *, #16407, .F. ) ;
#15233 = DIRECTION ( 'NONE',  ( -0.1566598588826321747, 0.9876526153536343555, 0.000000000000000000 ) ) ;
#15235 = CARTESIAN_POINT ( 'NONE',  ( -30.04042668367358360, -19.95224085582016116, -21.65063509461098334 ) ) ;
#15236 = VECTOR ( 'NONE', #16863, 1000.000000000000000 ) ;
#15237 = ORIENTED_EDGE ( 'NONE', *, *, #16230, .F. ) ;
#15238 = ORIENTED_EDGE ( 'NONE', *, *, #11658, .T. ) ;
#15239 = CARTESIAN_POINT ( 'NONE',  ( -56.21322099054477661, -24.10372711620990671, 4.330127018922218518 ) ) ;
#15240 =( REPRESENTATION_RELATIONSHIP ('NONE','NONE', #7353, #17876 ) REPRESENTATION_RELATIONSHIP_WITH_TRANSFORMATION ( #8377 )SHAPE_REPRESENTATION_RELATIONSHIP( ) );
#15241 = CARTESIAN_POINT ( 'NONE',  ( -30.69897130211303349, -82.82467515726038698, 8.660254037844412167 ) ) ;
#15242 = VERTEX_POINT ( 'NONE', #1655 ) ;
#15243 = FACE_OUTER_BOUND ( 'NONE', #8175, .T. ) ;
#15244 = CARTESIAN_POINT ( 'NONE',  ( -76.66445292623467367, -32.41017715895461038, -4.330127018922181215 ) ) ;
#15245 = DIRECTION ( 'NONE',  ( -0.9201637183752249260, -0.3915338189555018777, 0.000000000000000000 ) ) ;
#15246 = CARTESIAN_POINT ( 'NONE',  ( -169.4331498180839901, 31.75282987493100606, -2.500000000000000000 ) ) ;
#15247 = CARTESIAN_POINT ( 'NONE',  ( -47.32434745236209750, -22.69378838626622752, 8.660254037844417496 ) ) ;
#15248 = CARTESIAN_POINT ( 'NONE',  ( -84.16561914167408531, 33.59999999999999432, 30.00000000000000000 ) ) ;
#15249 = DIRECTION ( 'NONE',  ( -0.9876526153536336894, -0.1566598588826349503, 0.000000000000000000 ) ) ;
#15250 = DIRECTION ( 'NONE',  ( -0.9876526153536341335, -0.1566598588826327021, 0.000000000000000000 ) ) ;
#15251 = FILL_AREA_STYLE_COLOUR ( '', #18587 ) ;
#15252 = EDGE_CURVE ( 'NONE', #3698, #6795, #1525, .T. ) ;
#15253 = DIRECTION ( 'NONE',  ( -1.547359998875406858E-16, 4.084688078942370972E-17, -1.000000000000000000 ) ) ;
#15254 = ORIENTED_EDGE ( 'NONE', *, *, #2059, .F. ) ;
#15255 = DIRECTION ( 'NONE',  ( -0.9876526153536336894, -0.1566598588826350336, 0.000000000000000000 ) ) ;
#15256 = ORIENTED_EDGE ( 'NONE', *, *, #5714, .F. ) ;
#15257 = EDGE_CURVE ( 'NONE', #3679, #9221, #12694, .T. ) ;
#15258 = ORIENTED_EDGE ( 'NONE', *, *, #8811, .T. ) ;
#15259 = VERTEX_POINT ( 'NONE', #9029 ) ;
#15260 = CARTESIAN_POINT ( 'NONE',  ( -4.526176995241833367, -78.67318889687062722, -17.32050807568878525 ) ) ;
#15261 = FACE_BOUND ( 'NONE', #9090, .T. ) ;
#15262 = ORIENTED_EDGE ( 'NONE', *, *, #8870, .T. ) ;
#15263 = CARTESIAN_POINT ( 'NONE',  ( -129.1404785418517918, -2.850701963179328668, 12.74754878398196745 ) ) ;
#15264 = CIRCLE ( 'NONE', #17422, 1.499999999999999556 ) ;
#15265 = ORIENTED_EDGE ( 'NONE', *, *, #11715, .F. ) ;
#15266 = DIRECTION ( 'NONE',  ( -0.1566598588826321192, 0.9876526153536342445, 7.798540720466730171E-17 ) ) ;
#15267 = CARTESIAN_POINT ( 'NONE',  ( -71.02801022084922522, -26.45362499944938506, 12.99038105676661736 ) ) ;
#15268 = FACE_BOUND ( 'NONE', #6133, .T. ) ;
#15269 = DIRECTION ( 'NONE',  ( -0.1566598588826321192, 0.9876526153536342445, 7.798540720466731404E-17 ) ) ;
#15270 = ORIENTED_EDGE ( 'NONE', *, *, #960, .T. ) ;
#15271 = CYLINDRICAL_SURFACE ( 'NONE', #621, 1.500000000000001554 ) ;
#15272 = DIRECTION ( 'NONE',  ( 0.000000000000000000, 0.000000000000000000, 1.000000000000000000 ) ) ;
#15273 = DIRECTION ( 'NONE',  ( -0.1566598588826321747, 0.9876526153536343555, 0.000000000000000000 ) ) ;
#15274 = EDGE_CURVE ( 'NONE', #14342, #2732, #11773, .T. ) ;
#15275 = EDGE_LOOP ( 'NONE', ( #3090, #10129, #13202, #15460 ) ) ;
#15276 = ORIENTED_EDGE ( 'NONE', *, *, #15968, .F. ) ;
#15277 = CARTESIAN_POINT ( 'NONE',  ( -50.49165861936347710, -28.25869089856488614, 4.330127018922217630 ) ) ;
#15278 = ADVANCED_FACE ( 'NONE', ( #17494 ), #10263, .F. ) ;
#15279 = CIRCLE ( 'NONE', #18366, 1.499999999999999556 ) ;
#15280 = ADVANCED_FACE ( 'NONE', ( #16440 ), #16336, .F. ) ;
#15281 = CARTESIAN_POINT ( 'NONE',  ( -170.5817601278045288, 32.44591577653011427, -5.316095106350547717 ) ) ;
#15282 = ORIENTED_EDGE ( 'NONE', *, *, #12086, .T. ) ;
#15283 = ORIENTED_EDGE ( 'NONE', *, *, #280, .T. ) ;
#15284 = DIRECTION ( 'NONE',  ( -0.9876526153536341335, -0.1566598588826327021, 0.000000000000000000 ) ) ;
#15285 = ORIENTED_EDGE ( 'NONE', *, *, #17465, .F. ) ;
#15286 = DIRECTION ( 'NONE',  ( -0.9876526153536336894, -0.1566598588826349503, 0.000000000000000000 ) ) ;
#15287 = PRODUCT ( 'block pivot pin', 'block pivot pin', '', ( #8001 ) ) ;
#15288 = CARTESIAN_POINT ( 'NONE',  ( -39.09401853261887538, -84.15628395776273862, 8.660254037844412167 ) ) ;
#15289 = CIRCLE ( 'NONE', #7739, 1.500000000000000888 ) ;
#15290 = CARTESIAN_POINT ( 'NONE',  ( -71.72618984946653597, -31.62687786454144856, -12.99038105676658006 ) ) ;
#15291 = CARTESIAN_POINT ( 'NONE',  ( 73.09088021254186174, 1.387778780781445676E-14, -25.00000000000000000 ) ) ;
#15292 = DIRECTION ( 'NONE',  ( 0.4356311770055183996, 0.8863620251788737470, 0.1568050953942268233 ) ) ;
#15293 = DIRECTION ( 'NONE',  ( -0.1566598588826321192, 0.9876526153536342445, 7.798540720466730171E-17 ) ) ;
#15294 = DIRECTION ( 'NONE',  ( -0.9876526153536336894, -0.1566598588826349503, 0.000000000000000000 ) ) ;
#15295 = CARTESIAN_POINT ( 'NONE',  ( 0.3724510713484854851, -20.19070816610934926, 12.99038105676661026 ) ) ;
#15296 = DIRECTION ( 'NONE',  ( -8.693966348389027220E-17, 1.991237296706375196E-16, -1.000000000000000000 ) ) ;
#15297 = EDGE_CURVE ( 'NONE', #4549, #15692, #4824, .T. ) ;
#15298 = DIRECTION ( 'NONE',  ( -0.1566598588826321192, 0.9876526153536342445, 7.798540720466730171E-17 ) ) ;
#15299 = ORIENTED_EDGE ( 'NONE', *, *, #4469, .F. ) ;
#15300 = ORIENTED_EDGE ( 'NONE', *, *, #6249, .T. ) ;
#15301 = FACE_BOUND ( 'NONE', #15199, .T. ) ;
#15302 = DIRECTION ( 'NONE',  ( 0.000000000000000000, 0.000000000000000000, 1.000000000000000000 ) ) ;
#15303 = VERTEX_POINT ( 'NONE', #13189 ) ;
#15304 = AXIS2_PLACEMENT_3D ( 'NONE', #12470, #5278, #12360 ) ;
#15305 = ORIENTED_EDGE ( 'NONE', *, *, #15486, .F. ) ;
#15306 = ORIENTED_EDGE ( 'NONE', *, *, #9297, .F. ) ;
#15307 = EDGE_LOOP ( 'NONE', ( #3725, #828 ) ) ;
#15308 = EDGE_CURVE ( 'NONE', #3849, #859, #15436, .T. ) ;
#15309 = VERTEX_POINT ( 'NONE', #3145 ) ;
#15310 = AXIS2_PLACEMENT_3D ( 'NONE', #12870, #6061, #11977 ) ;
#15311 = ORIENTED_EDGE ( 'NONE', *, *, #3822, .T. ) ;
#15312 = DIRECTION ( 'NONE',  ( 0.000000000000000000, 0.000000000000000000, 1.000000000000000000 ) ) ;
#15313 = CARTESIAN_POINT ( 'NONE',  ( -8.476787456656362352, -79.29982833240116236, -4.330127018922185655 ) ) ;
#15314 = ORIENTED_EDGE ( 'NONE', *, *, #14335, .T. ) ;
#15315 = CARTESIAN_POINT ( 'NONE',  ( -176.1167811578620501, -139.6880237571007513, 2.500000000000000000 ) ) ;
#15316 = AXIS2_PLACEMENT_3D ( 'NONE', #18005, #16552, #13491 ) ;
#15317 = CARTESIAN_POINT ( 'NONE',  ( -57.69469991357522076, -24.33871690453386094, 21.65063509461101887 ) ) ;
#15318 = FACE_OUTER_BOUND ( 'NONE', #2044, .T. ) ;
#15319 =( NAMED_UNIT ( * ) SI_UNIT ( $, .STERADIAN. ) SOLID_ANGLE_UNIT ( ) );
#15320 = DIRECTION ( 'NONE',  ( -0.1566598588826321192, 0.9876526153536342445, 7.798540720466730171E-17 ) ) ;
#15321 = VECTOR ( 'NONE', #9179, 1000.000000000000000 ) ;
#15322 = DIRECTION ( 'NONE',  ( -0.1566598588826321192, 0.9876526153536342445, 7.798540720466730171E-17 ) ) ;
#15323 = CARTESIAN_POINT ( 'NONE',  ( 8.807133312032172867, -76.55828080195509244, -17.32050807568878525 ) ) ;
#15324 = CARTESIAN_POINT ( 'NONE',  ( -4.526176995241833367, -78.67318889687062722, 17.32050807568880657 ) ) ;
#15325 = ORIENTED_EDGE ( 'NONE', *, *, #15551, .T. ) ;
#15326 = DIRECTION ( 'NONE',  ( -0.000000000000000000, -0.000000000000000000, -1.000000000000000000 ) ) ;
#15327 = CIRCLE ( 'NONE', #11081, 1.500000000000000888 ) ;
#15328 = LINE ( 'NONE', #16878, #16325 ) ;
#15329 = ORIENTED_EDGE ( 'NONE', *, *, #9435, .F. ) ;
#15330 = EDGE_CURVE ( 'NONE', #11583, #18320, #14219, .T. ) ;
#15331 = DIRECTION ( 'NONE',  ( -0.1566598588826321192, 0.9876526153536342445, 7.798540720466731404E-17 ) ) ;
#15332 = EDGE_CURVE ( 'NONE', #12882, #16906, #8169, .T. ) ;
#15333 = AXIS2_PLACEMENT_3D ( 'NONE', #5169, #18384, #1024 ) ;
#15334 = DIRECTION ( 'NONE',  ( -0.1566598588826321192, 0.9876526153536342445, 7.798540720466730171E-17 ) ) ;
#15335 = AXIS2_PLACEMENT_3D ( 'NONE', #11716, #4540, #13428 ) ;
#15336 = EDGE_LOOP ( 'NONE', ( #1366, #2515 ) ) ;
#15337 = EDGE_CURVE ( 'NONE', #6519, #13656, #11661, .T. ) ;
#15338 = DIRECTION ( 'NONE',  ( 2.887450008416415878E-16, 0.000000000000000000, 1.000000000000000000 ) ) ;
#15339 = DIRECTION ( 'NONE',  ( -0.1566598588826321192, 0.9876526153536342445, 7.798540720466730171E-17 ) ) ;
#15340 = EDGE_LOOP ( 'NONE', ( #439, #11986 ) ) ;
#15341 = AXIS2_PLACEMENT_3D ( 'NONE', #6611, #6719, #15029 ) ;
#15342 = CARTESIAN_POINT ( 'NONE',  ( -29.05277406831996245, -19.79558099693753093, -17.32050807568878170 ) ) ;
#15343 = DIRECTION ( 'NONE',  ( 0.9826218788918642533, 0.1856185419698762884, -0.000000000000000000 ) ) ;
#15344 = AXIS2_PLACEMENT_3D ( 'NONE', #7018, #12761, #18613 ) ;
#15345 = DIRECTION ( 'NONE',  ( 0.000000000000000000, 0.000000000000000000, 1.000000000000000000 ) ) ;
#15346 = DIRECTION ( 'NONE',  ( -0.1566598588826321192, 0.9876526153536342445, 7.798540720466730171E-17 ) ) ;
#15347 = DIRECTION ( 'NONE',  ( 0.000000000000000000, 0.000000000000000000, 1.000000000000000000 ) ) ;
#15348 = DIRECTION ( 'NONE',  ( -0.1566598588826321192, 0.9876526153536342445, 7.798540720466730171E-17 ) ) ;
#15349 = ORIENTED_EDGE ( 'NONE', *, *, #16724, .F. ) ;
#15350 = DIRECTION ( 'NONE',  ( 0.000000000000000000, 0.000000000000000000, -1.000000000000000000 ) ) ;
#15351 = CIRCLE ( 'NONE', #14453, 1.500000000000000444 ) ;
#15352 = DIRECTION ( 'NONE',  ( -0.1566598588826321192, 0.9876526153536342445, 7.798540720466730171E-17 ) ) ;
#15353 = ORIENTED_EDGE ( 'NONE', *, *, #7664, .F. ) ;
#15354 = ORIENTED_EDGE ( 'NONE', *, *, #3556, .T. ) ;
#15355 = ORIENTED_EDGE ( 'NONE', *, *, #12910, .T. ) ;
#15356 = LINE ( 'NONE', #9294, #14722 ) ;
#15357 = VECTOR ( 'NONE', #16349, 1000.000000000000000 ) ;
#15358 = FACE_BOUND ( 'NONE', #4643, .T. ) ;
#15359 = EDGE_CURVE ( 'NONE', #5533, #9341, #7278, .T. ) ;
#15360 = CARTESIAN_POINT ( 'NONE',  ( 2.000000000000000000, 0.000000000000000000, -40.65685424949239035 ) ) ;
#15361 = EDGE_LOOP ( 'NONE', ( #14145, #9157, #13772, #2900 ) ) ;
#15362 = VECTOR ( 'NONE', #17230, 1000.000000000000000 ) ;
#15363 = DIRECTION ( 'NONE',  ( 0.000000000000000000, 0.000000000000000000, 1.000000000000000000 ) ) ;
#15364 = DIRECTION ( 'NONE',  ( 0.000000000000000000, 0.000000000000000000, 1.000000000000000000 ) ) ;
#15365 = EDGE_CURVE ( 'NONE', #3093, #18006, #6046, .T. ) ;
#15366 = CYLINDRICAL_SURFACE ( 'NONE', #18215, 1.500000000000001554 ) ;
#15367 = ORIENTED_EDGE ( 'NONE', *, *, #14027, .F. ) ;
#15368 = DIRECTION ( 'NONE',  ( -0.1566598588826321192, 0.9876526153536342445, 7.798540720466731404E-17 ) ) ;
#15369 = CYLINDRICAL_SURFACE ( 'NONE', #18152, 1.500000000000001554 ) ;
#15370 = DIRECTION ( 'NONE',  ( -0.9876526153536341335, -0.1566598588826327021, 0.000000000000000000 ) ) ;
#15371 = TOROIDAL_SURFACE ( 'NONE', #12018, 12.83663829214476060, 3.000000000000000000 ) ;
#15372 = ORIENTED_EDGE ( 'NONE', *, *, #8382, .F. ) ;
#15373 = FACE_OUTER_BOUND ( 'NONE', #12066, .T. ) ;
#15374 = ORIENTED_EDGE ( 'NONE', *, *, #15105, .T. ) ;
#15375 = DIRECTION ( 'NONE',  ( 0.000000000000000000, 0.000000000000000000, 1.000000000000000000 ) ) ;
#15376 = VECTOR ( 'NONE', #1249, 1000.000000000000000 ) ;
#15377 = CARTESIAN_POINT ( 'NONE',  ( -170.1316674247146352, 32.02951924490234603, -4.052748550462852428 ) ) ;
#15378 = VERTEX_POINT ( 'NONE', #14635 ) ;
#15379 = ORIENTED_EDGE ( 'NONE', *, *, #16123, .F. ) ;
#15380 = LINE ( 'NONE', #8288, #9743 ) ;
#15381 = EDGE_LOOP ( 'NONE', ( #15174, #3606 ) ) ;
#15382 = CARTESIAN_POINT ( 'NONE',  ( -52.96079015774756016, -28.65034054577145994, 8.660254037844417496 ) ) ;
#15383 = CYLINDRICAL_SURFACE ( 'NONE', #3000, 1.500000000000001554 ) ;
#15384 = EDGE_CURVE ( 'NONE', #11742, #1595, #6989, .T. ) ;
#15385 = FACE_BOUND ( 'NONE', #18324, .T. ) ;
#15386 = AXIS2_PLACEMENT_3D ( 'NONE', #1575, #8862, #7171 ) ;
#15387 = FACE_OUTER_BOUND ( 'NONE', #5187, .T. ) ;
#15388 = CIRCLE ( 'NONE', #14475, 15.83618137761394173 ) ;
#15389 = EDGE_CURVE ( 'NONE', #13798, #384, #3018, .T. ) ;
#15390 = CIRCLE ( 'NONE', #8451, 1.499999999999999556 ) ;
#15391 = DIRECTION ( 'NONE',  ( -0.1566598588826321192, 0.9876526153536342445, 7.798540720466730171E-17 ) ) ;
#15392 = EDGE_CURVE ( 'NONE', #1506, #12855, #3906, .T. ) ;
#15393 = CARTESIAN_POINT ( 'NONE',  ( -29.75095369693726610, -24.96883386202961574, 1.869203119972154228E-14 ) ) ;
#15394 = LINE ( 'NONE', #10828, #16565 ) ;
#15395 = FACE_OUTER_BOUND ( 'NONE', #9923, .T. ) ;
#15396 = VERTEX_POINT ( 'NONE', #507 ) ;
#15397 = EDGE_LOOP ( 'NONE', ( #924, #6112 ) ) ;
#15398 = CARTESIAN_POINT ( 'NONE',  ( 0.000000000000000000, 0.000000000000000000, 35.00000000000000000 ) ) ;
#15399 = DIRECTION ( 'NONE',  ( -0.1566598588826321192, 0.9876526153536342445, 7.798540720466730171E-17 ) ) ;
#15400 = AXIS2_PLACEMENT_3D ( 'NONE', #15561, #11644, #1367 ) ;
#15401 = ORIENTED_EDGE ( 'NONE', *, *, #12486, .T. ) ;
#15402 = EDGE_LOOP ( 'NONE', ( #13006, #16400, #14346, #252 ) ) ;
#15403 = AXIS2_PLACEMENT_3D ( 'NONE', #1519, #14402, #1428 ) ;
#15404 = CYLINDRICAL_SURFACE ( 'NONE', #11471, 20.00000000000001066 ) ;
#15405 = DIRECTION ( 'NONE',  ( -0.9876526153536344665, -0.1566598588826304539, 0.000000000000000000 ) ) ;
#15406 = CIRCLE ( 'NONE', #6349, 1.500000000000000888 ) ;
#15407 = ORIENTED_EDGE ( 'NONE', *, *, #1330, .F. ) ;
#15408 = ORIENTED_EDGE ( 'NONE', *, *, #8662, .F. ) ;
#15409 = DIRECTION ( 'NONE',  ( -0.1566598588826321192, 0.9876526153536342445, 7.798540720466730171E-17 ) ) ;
#15410 = CYLINDRICAL_SURFACE ( 'NONE', #15304, 1.500000000000001554 ) ;
#15411 = FACE_OUTER_BOUND ( 'NONE', #18541, .T. ) ;
#15412 = EDGE_CURVE ( 'NONE', #4575, #14954, #11858, .T. ) ;
#15413 = ORIENTED_EDGE ( 'NONE', *, *, #4171, .F. ) ;
#15414 = AXIS2_PLACEMENT_3D ( 'NONE', #8577, #12719, #14348 ) ;
#15415 = EDGE_CURVE ( 'NONE', #2, #12073, #8477, .T. ) ;
#15416 = CARTESIAN_POINT ( 'NONE',  ( 9.300959619709004755, -76.47995087251376845, 12.99038105676660493 ) ) ;
#15417 = ADVANCED_FACE ( 'NONE', ( #10904 ), #18271, .F. ) ;
#15418 = LINE ( 'NONE', #18011, #3720 ) ;
#15419 = CARTESIAN_POINT ( 'NONE',  ( -172.7326993491721225, 43.83249341393818810, 5.500000000000000000 ) ) ;
#15420 = CIRCLE ( 'NONE', #10565, 2.199999999999993516 ) ;
#15421 = CIRCLE ( 'NONE', #4815, 2.500000000000002220 ) ;
#15422 = CARTESIAN_POINT ( 'NONE',  ( -25.10216360690543524, -19.16894156140701710, 21.65063509461101887 ) ) ;
#15423 = AXIS2_PLACEMENT_3D ( 'NONE', #2558, #976, #18141 ) ;
#15424 = AXIS2_PLACEMENT_3D ( 'NONE', #5164, #8089, #10926 ) ;
#15425 = VERTEX_POINT ( 'NONE', #12429 ) ;
#15426 = CARTESIAN_POINT ( 'NONE',  ( 73.09088021254186174, 1.387778780781445676E-14, 25.00000000000000000 ) ) ;
#15427 = DIRECTION ( 'NONE',  ( -0.1566598588826321192, 0.9876526153536342445, 7.798540720466731404E-17 ) ) ;
#15428 = ORIENTED_EDGE ( 'NONE', *, *, #6296, .F. ) ;
#15429 = CARTESIAN_POINT ( 'NONE',  ( -81.09522717867928066, 30.58561221855817891, 35.00001199999999812 ) ) ;
#15430 = CARTESIAN_POINT ( 'NONE',  ( -67.07739975943471222, -25.82698556391885703, 1.926565525561698076E-14 ) ) ;
#15432 = ORIENTED_EDGE ( 'NONE', *, *, #5264, .T. ) ;
#15431 = DIRECTION ( 'NONE',  ( 0.1856185419698762329, -0.9826218788918640312, 0.000000000000000000 ) ) ;
#15433 = AXIS2_PLACEMENT_3D ( 'NONE', #2733, #8525, #1332 ) ;
#15434 = DIRECTION ( 'NONE',  ( 1.000000000000000000, 0.000000000000000000, -2.631994239413086031E-16 ) ) ;
#15435 = DIRECTION ( 'NONE',  ( -0.000000000000000000, -0.000000000000000000, -1.000000000000000000 ) ) ;
#15436 = CIRCLE ( 'NONE', #4534, 1.500000000000000888 ) ;
#15437 = EDGE_LOOP ( 'NONE', ( #11547, #11959, #8210, #7069 ) ) ;
#15438 = ORIENTED_EDGE ( 'NONE', *, *, #4573, .T. ) ;
#15439 = VERTEX_POINT ( 'NONE', #17974 ) ;
#15440 = AXIS2_PLACEMENT_3D ( 'NONE', #11954, #17800, #10561 ) ;
#15441 = CIRCLE ( 'NONE', #5772, 2.500000000000002220 ) ;
#15442 = CYLINDRICAL_SURFACE ( 'NONE', #1577, 1.500000000000001554 ) ;
#15443 = VERTEX_POINT ( 'NONE', #2109 ) ;
#15444 = DIRECTION ( 'NONE',  ( -0.1566598588826321192, 0.9876526153536342445, 7.798540720466731404E-17 ) ) ;
#15445 = CARTESIAN_POINT ( 'NONE',  ( -6.326550248787502032E-15, 2.311308694482618949E-14, -130.3485206753969976 ) ) ;
#15446 = CARTESIAN_POINT ( 'NONE',  ( -66.25446545484369665, -88.46443007703511796, 21.65063509461101532 ) ) ;
#15447 = CIRCLE ( 'NONE', #16056, 1.500000000000000888 ) ;
#15448 = CARTESIAN_POINT ( 'NONE',  ( 7.819480696678551723, -76.71494066083772623, 21.65063509461100821 ) ) ;
#15449 = CARTESIAN_POINT ( 'NONE',  ( 2.881217619910392269, -77.49823995525089515, 12.99038105676660493 ) ) ;
#15450 = DIRECTION ( 'NONE',  ( -0.9876526153536336894, -0.1566598588826349503, 0.000000000000000000 ) ) ;
#15451 = ORIENTED_EDGE ( 'NONE', *, *, #4019, .F. ) ;
#15452 = FACE_OUTER_BOUND ( 'NONE', #16504, .T. ) ;
#15453 = FACE_BOUND ( 'NONE', #4602, .T. ) ;
#15454 = ADVANCED_FACE ( 'NONE', ( #11087 ), #15271, .F. ) ;
#15455 = CIRCLE ( 'NONE', #6068, 1.499999999999999556 ) ;
#15456 = EDGE_CURVE ( 'NONE', #3230, #10291, #918, .T. ) ;
#15457 = AXIS2_PLACEMENT_3D ( 'NONE', #5178, #3918, #15405 ) ;
#15458 = ORIENTED_EDGE ( 'NONE', *, *, #13722, .F. ) ;
#15459 = DIRECTION ( 'NONE',  ( -0.9876526153536341335, -0.1566598588826327021, 0.000000000000000000 ) ) ;
#15460 = ORIENTED_EDGE ( 'NONE', *, *, #2556, .T. ) ;
#15461 = VERTEX_POINT ( 'NONE', #3785 ) ;
#15462 = CIRCLE ( 'NONE', #7307, 1.499999999999999556 ) ;
#15463 = DIRECTION ( 'NONE',  ( -0.1566598588826321192, 0.9876526153536342445, 7.798540720466730171E-17 ) ) ;
#15464 = VECTOR ( 'NONE', #16465, 1000.000000000000000 ) ;
#15465 = FACE_BOUND ( 'NONE', #12947, .T. ) ;
#15466 = CARTESIAN_POINT ( 'NONE',  ( -28.26947477390680774, -24.73384407370567217, 8.660254037844417496 ) ) ;
#15467 = EDGE_LOOP ( 'NONE', ( #12188, #9714, #8942, #541 ) ) ;
#15468 = CIRCLE ( 'NONE', #6087, 2.200000000000000178 ) ;
#15469 = DIRECTION ( 'NONE',  ( -0.000000000000000000, -0.000000000000000000, -1.000000000000000000 ) ) ;
#15470 = ORIENTED_EDGE ( 'NONE', *, *, #13023, .T. ) ;
#15472 = EDGE_CURVE ( 'NONE', #537, #10340, #13842, .T. ) ;
#15471 = CARTESIAN_POINT ( 'NONE',  ( 2.841582609732560272, -19.79905851890276836, -8.660254037844383745 ) ) ;
#15473 = DIRECTION ( 'NONE',  ( 0.000000000000000000, 0.000000000000000000, 1.000000000000000000 ) ) ;
#15474 = CARTESIAN_POINT ( 'NONE',  ( 73.09088021254186174, 1.387778780781445676E-14, 7.500000000000000000 ) ) ;
#15475 = CARTESIAN_POINT ( 'NONE',  ( -44.07191661956487394, -27.24040181582776299, 12.99038105676661736 ) ) ;
#15476 = ORIENTED_EDGE ( 'NONE', *, *, #18751, .F. ) ;
#15477 = DIRECTION ( 'NONE',  ( 1.000000000000000000, 0.000000000000000000, 0.000000000000000000 ) ) ;
#15478 = EDGE_CURVE ( 'NONE', #1662, #1326, #7563, .T. ) ;
#15479 = CARTESIAN_POINT ( 'NONE',  ( -56.37793930130739994, -86.89783148820880854, 21.65063509461101532 ) ) ;
#15480 = CARTESIAN_POINT ( 'NONE',  ( -49.95819730150881099, -85.87954240547166762, -12.99038105676658539 ) ) ;
#15481 = CIRCLE ( 'NONE', #13048, 1.499999999999999556 ) ;
#15482 = ORIENTED_EDGE ( 'NONE', *, *, #18102, .T. ) ;
#15483 = EDGE_LOOP ( 'NONE', ( #181, #102, #13492, #5906 ) ) ;
#15484 = DIRECTION ( 'NONE',  ( -0.9876526153536341335, -0.1566598588826327021, 0.000000000000000000 ) ) ;
#15485 = CARTESIAN_POINT ( 'NONE',  ( -70.24471092643608472, -31.39188807621751209, -4.330127018922181215 ) ) ;
#15486 = EDGE_CURVE ( 'NONE', #4436, #18590, #2118, .T. ) ;
#15487 = AXIS2_PLACEMENT_3D ( 'NONE', #11967, #1605, #7742 ) ;
#15488 = CIRCLE ( 'NONE', #15187, 1.500000000000000888 ) ;
#15489 = LINE ( 'NONE', #14056, #9427 ) ;
#15490 = AXIS2_PLACEMENT_3D ( 'NONE', #7034, #12781, #18626 ) ;
#15491 = DIRECTION ( 'NONE',  ( -0.1566598588826321192, 0.9876526153536342445, 7.798540720466731404E-17 ) ) ;
#15492 = DIRECTION ( 'NONE',  ( -0.1566598588826321192, 0.9876526153536342445, 7.798540720466730171E-17 ) ) ;
#15493 = DIRECTION ( 'NONE',  ( -0.1566598588826321192, 0.9876526153536342445, 7.798540720466730171E-17 ) ) ;
#15494 = CARTESIAN_POINT ( 'NONE',  ( -65.23030399291528170, -43.49999999999991473, -19.99999999999999645 ) ) ;
#15495 = VECTOR ( 'NONE', #6365, 1000.000000000000000 ) ;
#15496 = DIRECTION ( 'NONE',  ( -0.1566598588826321192, 0.9876526153536342445, 7.798540720466730171E-17 ) ) ;
#15497 = DIRECTION ( 'NONE',  ( -0.9876526153536341335, -0.1566598588826327021, 0.000000000000000000 ) ) ;
#15498 = DIRECTION ( 'NONE',  ( -0.9876526153536341335, -0.1566598588826327021, 0.000000000000000000 ) ) ;
#15499 = MECHANICAL_DESIGN_GEOMETRIC_PRESENTATION_REPRESENTATION (  '', ( #13069 ), #16118 ) ;
#15500 = DIRECTION ( 'NONE',  ( 0.000000000000000000, 0.000000000000000000, 1.000000000000000000 ) ) ;
#15501 = ORIENTED_EDGE ( 'NONE', *, *, #10077, .F. ) ;
#15502 = ORIENTED_EDGE ( 'NONE', *, *, #10161, .F. ) ;
#15503 = CARTESIAN_POINT ( 'NONE',  ( -46.50141314777110324, -85.33123289938248490, 4.330127018922213189 ) ) ;
#15504 = EDGE_CURVE ( 'NONE', #17370, #5489, #1000, .T. ) ;
#15505 = EDGE_LOOP ( 'NONE', ( #12568, #5703 ) ) ;
#15506 = AXIS2_PLACEMENT_3D ( 'NONE', #8403, #3738, #12371 ) ;
#15507 = DIRECTION ( 'NONE',  ( 0.000000000000000000, 0.000000000000000000, 1.000000000000000000 ) ) ;
#15508 = EDGE_LOOP ( 'NONE', ( #10691, #11221 ) ) ;
#15509 = CARTESIAN_POINT ( 'NONE',  ( -8.516422466834198346, -21.60064689605303911, 8.660254037844413944 ) ) ;
#15510 = EDGE_CURVE ( 'NONE', #15004, #13436, #7983, .T. ) ;
#15511 = VERTEX_POINT ( 'NONE', #16727 ) ;
#15512 = DIRECTION ( 'NONE',  ( 0.000000000000000000, 0.000000000000000000, 1.000000000000000000 ) ) ;
#15513 = DIRECTION ( 'NONE',  ( 0.000000000000000000, 0.000000000000000000, -1.000000000000000000 ) ) ;
#15514 = DIRECTION ( 'NONE',  ( -0.9826218788918642533, -0.1856185419698762884, 0.000000000000000000 ) ) ;
#15515 = CYLINDRICAL_SURFACE ( 'NONE', #5836, 1.500000000000001554 ) ;
#15516 = SURFACE_STYLE_FILL_AREA ( #943 ) ;
#15517 = PRESENTATION_LAYER_ASSIGNMENT (  '', '', ( #4001 ) ) ;
#15518 = CARTESIAN_POINT ( 'NONE',  ( -24.27922930231443743, -81.80638607452326028, -17.32050807568878525 ) ) ;
#15519 = CARTESIAN_POINT ( 'NONE',  ( -9.299721761247353058, -16.66238381928489787, 17.32050807568881368 ) ) ;
#15520 = LINE ( 'NONE', #3837, #16889 ) ;
#15521 = ORIENTED_EDGE ( 'NONE', *, *, #2967, .F. ) ;
#15522 = CARTESIAN_POINT ( 'NONE',  ( -26.58364252993588650, -19.40393134973095357, -4.330127018922180326 ) ) ;
#15523 = CARTESIAN_POINT ( 'NONE',  ( -78.35789227062710438, 0.9448366394476784835, 3.952811421308334072 ) ) ;
#15524 = ORIENTED_EDGE ( 'NONE', *, *, #8539, .F. ) ;
#15525 = EDGE_CURVE ( 'NONE', #10629, #18301, #1240, .T. ) ;
#15526 = EDGE_CURVE ( 'NONE', #12710, #14627, #18361, .T. ) ;
#15527 = DIRECTION ( 'NONE',  ( -1.000000000000000000, 0.000000000000000000, 0.000000000000000000 ) ) ;
#15528 = EDGE_LOOP ( 'NONE', ( #17589, #3446 ) ) ;
#15529 = EDGE_CURVE ( 'NONE', #15709, #5881, #13296, .T. ) ;
#15530 = CIRCLE ( 'NONE', #5856, 1.500000000000001332 ) ;
#15531 = EDGE_CURVE ( 'NONE', #13656, #12208, #15731, .T. ) ;
#15532 = CARTESIAN_POINT ( 'NONE',  ( -19.38060123572413218, -23.32390534376198232, -4.330127018922181215 ) ) ;
#15533 = EDGE_LOOP ( 'NONE', ( #756, #4859, #471, #16298 ) ) ;
#15534 = DIRECTION ( 'NONE',  ( 0.000000000000000000, 0.000000000000000000, 1.000000000000000000 ) ) ;
#15535 = CARTESIAN_POINT ( 'NONE',  ( -128.5628356445764382, 9.332895270846938374, -3.719291248522909488 ) ) ;
#15536 = FACE_OUTER_BOUND ( 'NONE', #8407, .T. ) ;
#15537 = DIRECTION ( 'NONE',  ( -0.000000000000000000, -0.000000000000000000, -1.000000000000000000 ) ) ;
#15538 = CARTESIAN_POINT ( 'NONE',  ( -56.37793930130741415, -86.89783148820879433, 4.330127018922213189 ) ) ;
#15539 = FACE_OUTER_BOUND ( 'NONE', #668, .T. ) ;
#15540 = CYLINDRICAL_SURFACE ( 'NONE', #17354, 1.500000000000001554 ) ;
#15541 = CARTESIAN_POINT ( 'NONE',  ( -21.84973277410820458, -23.71555499096855613, 17.32050807568881723 ) ) ;
#15542 = VECTOR ( 'NONE', #17269, 1000.000000000000000 ) ;
#15543 = ORIENTED_EDGE ( 'NONE', *, *, #13553, .T. ) ;
#15544 = EDGE_CURVE ( 'NONE', #14684, #1532, #9975, .T. ) ;
#15545 = FACE_OUTER_BOUND ( 'NONE', #17394, .T. ) ;
#15546 = ORIENTED_EDGE ( 'NONE', *, *, #3716, .F. ) ;
#15547 = VERTEX_POINT ( 'NONE', #12133 ) ;
#15548 = CARTESIAN_POINT ( 'NONE',  ( -20.82244514857674389, -81.25807656843406335, -8.660254037844385522 ) ) ;
#15549 = FACE_BOUND ( 'NONE', #377, .T. ) ;
#15550 = EDGE_CURVE ( 'NONE', #7797, #3315, #2288, .T. ) ;
#15551 = EDGE_CURVE ( 'NONE', #17451, #8575, #10803, .T. ) ;
#15552 = DIRECTION ( 'NONE',  ( 0.000000000000000000, 0.000000000000000000, 1.000000000000000000 ) ) ;
#15553 = CARTESIAN_POINT ( 'NONE',  ( 0.4120860815263194254, -77.88988960245745830, -17.32050807568878525 ) ) ;
#15554 = VERTEX_POINT ( 'NONE', #8070 ) ;
#15555 = CARTESIAN_POINT ( 'NONE',  ( -50.45202360918564466, -85.95787233491300583, -8.660254037844385522 ) ) ;
#15556 = VERTEX_POINT ( 'NONE', #701 ) ;
#15557 = DIRECTION ( 'NONE',  ( -0.1566598588826321192, 0.9876526153536342445, 7.798540720466730171E-17 ) ) ;
#15558 = DIRECTION ( 'NONE',  ( 1.438274729681541867E-16, 6.252920376642369977E-17, -1.000000000000000000 ) ) ;
#15559 = DIRECTION ( 'NONE',  ( -0.1566598588826321192, 0.9876526153536342445, 7.798540720466730171E-17 ) ) ;
#15560 = DIRECTION ( 'NONE',  ( -0.1566598588826321192, 0.9876526153536342445, 7.798540720466731404E-17 ) ) ;
#15561 = CARTESIAN_POINT ( 'NONE',  ( -3.578159390066044665, -20.81734760163988440, 17.32050807568881012 ) ) ;
#15562 = EDGE_LOOP ( 'NONE', ( #9531, #15818, #735, #5069 ) ) ;
#15563 = ORIENTED_EDGE ( 'NONE', *, *, #5189, .T. ) ;
#15564 = EDGE_LOOP ( 'NONE', ( #3245, #8112, #2437, #13162 ) ) ;
#15565 = DIRECTION ( 'NONE',  ( -0.1566598588826321192, 0.9876526153536342445, 7.798540720466730171E-17 ) ) ;
#15566 = ORIENTED_EDGE ( 'NONE', *, *, #9783, .F. ) ;
#15567 = ORIENTED_EDGE ( 'NONE', *, *, #2432, .T. ) ;
#15568 = CARTESIAN_POINT ( 'NONE',  ( -129.0548615328497419, -14.67457578939283103, 4.764204982952881196 ) ) ;
#15569 = EDGE_CURVE ( 'NONE', #1993, #8675, #18061, .T. ) ;
#15570 = DIRECTION ( 'NONE',  ( -0.1566598588826321192, 0.9876526153536342445, 7.798540720466730171E-17 ) ) ;
#15571 = EDGE_LOOP ( 'NONE', ( #15607, #17555 ) ) ;
#15572 = EDGE_CURVE ( 'NONE', #11621, #5655, #3603, .T. ) ;
#15573 = CARTESIAN_POINT ( 'NONE',  ( -70.00000000000002842, 45.00000000000000711, 7.169068164496141371 ) ) ;
#15574 = DIRECTION ( 'NONE',  ( -0.000000000000000000, 1.000000000000000000, -0.000000000000000000 ) ) ;
#15575 = CIRCLE ( 'NONE', #14972, 145.0000000000000284 ) ;
#15576 = FACE_OUTER_BOUND ( 'NONE', #10739, .T. ) ;
#15577 = ORIENTED_EDGE ( 'NONE', *, *, #6391, .T. ) ;
#15578 = FACE_OUTER_BOUND ( 'NONE', #10040, .T. ) ;
#15579 = DIRECTION ( 'NONE',  ( 0.000000000000000000, -1.445602896647338917E-16, 1.000000000000000000 ) ) ;
#15580 = ORIENTED_EDGE ( 'NONE', *, *, #7358, .T. ) ;
#15581 = ORIENTED_EDGE ( 'NONE', *, *, #6335, .F. ) ;
#15582 = DIRECTION ( 'NONE',  ( -0.1566598588826321470, 0.9876526153536342445, 0.000000000000000000 ) ) ;
#15583 = LINE ( 'NONE', #10937, #1849 ) ;
#15584 = ORIENTED_EDGE ( 'NONE', *, *, #5918, .F. ) ;
#15585 = CYLINDRICAL_SURFACE ( 'NONE', #301, 1.500000000000001554 ) ;
#15586 = ORIENTED_EDGE ( 'NONE', *, *, #15486, .T. ) ;
#15587 = DIRECTION ( 'NONE',  ( -0.1566598588826321192, 0.9876526153536342445, 7.798540720466730171E-17 ) ) ;
#15588 = VECTOR ( 'NONE', #15212, 1000.000000000000000 ) ;
#15589 = CARTESIAN_POINT ( 'NONE',  ( -62.13913668266656032, -25.04368626950569876, 1.926565525561698076E-14 ) ) ;
#15590 = ORIENTED_EDGE ( 'NONE', *, *, #7249, .T. ) ;
#15591 = CYLINDRICAL_SURFACE ( 'NONE', #3047, 1.500000000000000666 ) ;
#15592 = ADVANCED_FACE ( 'NONE', ( #5137 ), #10144, .F. ) ;
#15593 = CARTESIAN_POINT ( 'NONE',  ( 55.85952145814821534, 6.938893903907228378E-15, 92.77853496600735639 ) ) ;
#15594 = FACE_OUTER_BOUND ( 'NONE', #7486, .T. ) ;
#15595 =( NAMED_UNIT ( * ) SI_UNIT ( $, .STERADIAN. ) SOLID_ANGLE_UNIT ( ) );
#15596 =( REPRESENTATION_RELATIONSHIP ('NONE','NONE', #7353, #13723 ) REPRESENTATION_RELATIONSHIP_WITH_TRANSFORMATION ( #1381 )SHAPE_REPRESENTATION_RELATIONSHIP( ) );
#15597 = FACE_OUTER_BOUND ( 'NONE', #18281, .T. ) ;
#15598 = FACE_OUTER_BOUND ( 'NONE', #1504, .T. ) ;
#15599 = ADVANCED_FACE ( 'NONE', ( #4372 ), #6964, .F. ) ;
#15600 = DIRECTION ( 'NONE',  ( -0.1566598588826321192, 0.9876526153536342445, 7.798540720466731404E-17 ) ) ;
#15601 = PLANE ( 'NONE',  #11674 ) ;
#15602 = ORIENTED_EDGE ( 'NONE', *, *, #14660, .F. ) ;
#15603 = CARTESIAN_POINT ( 'NONE',  ( -82.64970099990441099, 30.67540679198930320, 35.00001199999999812 ) ) ;
#15604 = DIRECTION ( 'NONE',  ( -0.1566598588826321192, 0.9876526153536342445, 7.798540720466730171E-17 ) ) ;
#15605 = ORIENTED_EDGE ( 'NONE', *, *, #11422, .F. ) ;
#15606 = LINE ( 'NONE', #8417, #7882 ) ;
#15607 = ORIENTED_EDGE ( 'NONE', *, *, #11571, .T. ) ;
#15608 = VERTEX_POINT ( 'NONE', #9790 ) ;
#15609 = ORIENTED_EDGE ( 'NONE', *, *, #11792, .T. ) ;
#15610 = CIRCLE ( 'NONE', #9560, 12.74754878398197633 ) ;
#15611 = CARTESIAN_POINT ( 'NONE',  ( -169.4331498180839901, 31.75282987493098474, 2.500000000000000000 ) ) ;
#15612 = CARTESIAN_POINT ( 'NONE',  ( -347.2219194661251436, -2.192405777922094678, 9.951701414186830458E-16 ) ) ;
#15613 = CARTESIAN_POINT ( 'NONE',  ( -33.99103714508810725, -20.57888029135068919, -8.660254037844380193 ) ) ;
#15614 = AXIS2_PLACEMENT_3D ( 'NONE', #10034, #94, #12960 ) ;
#15615 = CARTESIAN_POINT ( 'NONE',  ( 0.000000000000000000, 0.000000000000000000, -22.00000000000000711 ) ) ;
#15616 = DIRECTION ( 'NONE',  ( -0.1566598588826321192, 0.9876526153536342445, 7.798540720466730171E-17 ) ) ;
#15617 = ADVANCED_FACE ( 'NONE', ( #12604 ), #4284, .F. ) ;
#15618 = ADVANCED_FACE ( 'NONE', ( #11188 ), #15933, .F. ) ;
#15619 = CARTESIAN_POINT ( 'NONE',  ( -48.02252708097940825, -27.86704125135830523, 1.869203119972154228E-14 ) ) ;
#15620 = DIRECTION ( 'NONE',  ( -0.000000000000000000, -0.000000000000000000, -1.000000000000000000 ) ) ;
#15621 = ADVANCED_FACE ( 'NONE', ( #2941 ), #12703, .F. ) ;
#15622 = DIRECTION ( 'NONE',  ( -1.000000000000000000, 0.000000000000000000, -3.816390434826605238E-17 ) ) ;
#15623 = DIRECTION ( 'NONE',  ( 0.1856185419698762329, -0.9826218788918640312, 0.000000000000000000 ) ) ;
#15624 = AXIS2_PLACEMENT_3D ( 'NONE', #10794, #12721, #8085 ) ;
#15625 = ORIENTED_EDGE ( 'NONE', *, *, #9575, .T. ) ;
#15626 = ORIENTED_EDGE ( 'NONE', *, *, #6849, .T. ) ;
#15627 = ORIENTED_EDGE ( 'NONE', *, *, #9439, .F. ) ;
#15628 = CARTESIAN_POINT ( 'NONE',  ( -62.00000000000000000, 0.000000000000000000, -25.00000000000000000 ) ) ;
#15629 = AXIS2_PLACEMENT_3D ( 'NONE', #11323, #18611, #14188 ) ;
#15630 = EDGE_LOOP ( 'NONE', ( #6511, #9691, #1603, #2190 ) ) ;
#15631 = ORIENTED_EDGE ( 'NONE', *, *, #18277, .T. ) ;
#15632 = DIRECTION ( 'NONE',  ( -0.1566598588826321747, 0.9876526153536343555, 0.000000000000000000 ) ) ;
#15633 = DIRECTION ( 'NONE',  ( -0.1566598588826321192, 0.9876526153536342445, 7.798540720466731404E-17 ) ) ;
#15634 = VECTOR ( 'NONE', #1324, 1000.000000000000000 ) ;
#15635 = AXIS2_PLACEMENT_3D ( 'NONE', #6074, #4544, #1978 ) ;
#15636 = CARTESIAN_POINT ( 'NONE',  ( -42.55080268635659735, -84.70459346385193555, -17.32050807568878525 ) ) ;
#15637 = EDGE_LOOP ( 'NONE', ( #4267, #907, #18196, #4840 ) ) ;
#15638 = EDGE_CURVE ( 'NONE', #17453, #4620, #629, .T. ) ;
#15639 = ADVANCED_FACE ( 'NONE', ( #4075 ), #14039, .F. ) ;
#15640 = AXIS2_PLACEMENT_3D ( 'NONE', #16844, #7922, #13680 ) ;
#15641 = ORIENTED_EDGE ( 'NONE', *, *, #16806, .T. ) ;
#15642 = ORIENTED_EDGE ( 'NONE', *, *, #1444, .F. ) ;
#15643 = FACE_OUTER_BOUND ( 'NONE', #7129, .T. ) ;
#15644 = DIRECTION ( 'NONE',  ( -0.1566598588826321192, 0.9876526153536342445, 7.798540720466730171E-17 ) ) ;
#15645 = CARTESIAN_POINT ( 'NONE',  ( 6.831828081324923474, -76.87160051972034580, -8.660254037844389075 ) ) ;
#15646 = AXIS2_PLACEMENT_3D ( 'NONE', #5201, #3747, #12088 ) ;
#15647 = CARTESIAN_POINT ( 'NONE',  ( -39.09401853261887538, -84.15628395776273862, 8.660254037844412167 ) ) ;
#15648 = VERTEX_POINT ( 'NONE', #9871 ) ;
#15649 = ORIENTED_EDGE ( 'NONE', *, *, #10295, .T. ) ;
#15650 = ORIENTED_EDGE ( 'NONE', *, *, #5158, .T. ) ;
#15651 = ORIENTED_EDGE ( 'NONE', *, *, #4288, .F. ) ;
#15652 = CYLINDRICAL_SURFACE ( 'NONE', #12435, 1.500000000000001554 ) ;
#15653 = VERTEX_POINT ( 'NONE', #18460 ) ;
#15654 = EDGE_LOOP ( 'NONE', ( #6947, #6959, #1333, #18138 ) ) ;
#15655 = DIRECTION ( 'NONE',  ( -0.1566598588826321192, 0.9876526153536342445, 7.798540720466731404E-17 ) ) ;
#15656 = AXIS2_PLACEMENT_3D ( 'NONE', #622, #12145, #16163 ) ;
#15657 = DIRECTION ( 'NONE',  ( -2.735665993912342121E-16, -0.000000000000000000, -1.000000000000000000 ) ) ;
#15658 = DIRECTION ( 'NONE',  ( -0.1566598588826321192, 0.9876526153536342445, 7.798540720466730171E-17 ) ) ;
#15659 = DIRECTION ( 'NONE',  ( 0.000000000000000000, 0.000000000000000000, 1.000000000000000000 ) ) ;
#15660 = DIRECTION ( 'NONE',  ( 0.000000000000000000, 0.000000000000000000, 1.000000000000000000 ) ) ;
#15661 = DIRECTION ( 'NONE',  ( -8.693966348389027220E-17, 1.991237296706375196E-16, -1.000000000000000000 ) ) ;
#15662 = CONTEXT_DEPENDENT_SHAPE_REPRESENTATION ( #5209, #14261 ) ;
#15663 = VERTEX_POINT ( 'NONE', #17012 ) ;
#15664 = DIRECTION ( 'NONE',  ( -0.1566598588826321747, 0.9876526153536343555, 0.000000000000000000 ) ) ;
#15665 = CARTESIAN_POINT ( 'NONE',  ( -1.892327146095121204, -15.48743487766515337, 21.65063509461101532 ) ) ;
#15666 = ORIENTED_EDGE ( 'NONE', *, *, #2102, .T. ) ;
#15667 = EDGE_CURVE ( 'NONE', #7992, #3794, #12709, .T. ) ;
#15668 = CIRCLE ( 'NONE', #1461, 1.499999999999999556 ) ;
#15669 = DIRECTION ( 'NONE',  ( -0.9876526153536336894, -0.1566598588826350336, 0.000000000000000000 ) ) ;
#15670 = DIRECTION ( 'NONE',  ( 0.000000000000000000, 1.000000000000000000, 0.000000000000000000 ) ) ;
#15671 = ORIENTED_EDGE ( 'NONE', *, *, #3770, .F. ) ;
#15672 = EDGE_CURVE ( 'NONE', #12329, #9759, #3924, .T. ) ;
#15673 = ORIENTED_EDGE ( 'NONE', *, *, #4550, .T. ) ;
#15674 = DIRECTION ( 'NONE',  ( -0.9868632313631133801, 0.1615579233078772436, -0.000000000000000000 ) ) ;
#15675 = CARTESIAN_POINT ( 'NONE',  ( -66.25446545484369665, -88.46443007703511796, 4.330127018922213189 ) ) ;
#15676 = VERTEX_POINT ( 'NONE', #14241 ) ;
#15677 = SHAPE_REPRESENTATION ( 'block pivot pin', ( #18772 ), #13228 ) ;
#15678 = EDGE_CURVE ( 'NONE', #8415, #8214, #17389, .T. ) ;
#15679 = DIRECTION ( 'NONE',  ( -0.9876526153536341335, -0.1566598588826327021, 0.000000000000000000 ) ) ;
#15680 = EDGE_LOOP ( 'NONE', ( #10221, #14116, #8079, #16295 ) ) ;
#15681 = ORIENTED_EDGE ( 'NONE', *, *, #1546, .F. ) ;
#15682 = AXIS2_PLACEMENT_3D ( 'NONE', #17702, #3513, #17980 ) ;
#15683 = VERTEX_POINT ( 'NONE', #1088 ) ;
#15684 = CYLINDRICAL_SURFACE ( 'NONE', #2757, 1.500000000000001554 ) ;
#15685 = VECTOR ( 'NONE', #2796, 1000.000000000000000 ) ;
#15686 = VECTOR ( 'NONE', #9872, 1000.000000000000000 ) ;
#15687 = LINE ( 'NONE', #12747, #12387 ) ;
#15688 = AXIS2_PLACEMENT_3D ( 'NONE', #9176, #3273, #8970 ) ;
#15689 = DIRECTION ( 'NONE',  ( 0.000000000000000000, 0.000000000000000000, 1.000000000000000000 ) ) ;
#15690 = CARTESIAN_POINT ( 'NONE',  ( 2.000000000000000000, 2.449293598294706414E-16, 30.00000000000000000 ) ) ;
#15691 = DIRECTION ( 'NONE',  ( -0.1566598588826321192, 0.9876526153536342445, 7.798540720466730171E-17 ) ) ;
#15692 = VERTEX_POINT ( 'NONE', #17198 ) ;
#15693 = PLANE ( 'NONE',  #18453 ) ;
#15695 = DIRECTION ( 'NONE',  ( 0.000000000000000000, 0.000000000000000000, 1.000000000000000000 ) ) ;
#15694 = CIRCLE ( 'NONE', #7534, 1.500000000000000888 ) ;
#15696 = CARTESIAN_POINT ( 'NONE',  ( -309.1404785418517918, -2.850701963179328668, 9.951701414186818625E-16 ) ) ;
#15697 = VECTOR ( 'NONE', #5690, 1000.000000000000000 ) ;
#15698 = DIRECTION ( 'NONE',  ( 0.000000000000000000, 0.000000000000000000, 1.000000000000000000 ) ) ;
#15699 = ORIENTED_EDGE ( 'NONE', *, *, #12484, .F. ) ;
#15700 = CARTESIAN_POINT ( 'NONE',  ( -41.60278508118080509, -26.84875216862118918, -8.660254037844380193 ) ) ;
#15701 = AXIS2_PLACEMENT_3D ( 'NONE', #14359, #16153, #3147 ) ;
#15703 = VERTEX_POINT ( 'NONE', #1279 ) ;
#15702 = CARTESIAN_POINT ( 'NONE',  ( -41.56315007100295844, -84.54793360496931598, -4.330127018922185655 ) ) ;
#15704 = ORIENTED_EDGE ( 'NONE', *, *, #444, .F. ) ;
#15705 = EDGE_CURVE ( 'NONE', #5872, #12885, #29, .T. ) ;
#15706 = CARTESIAN_POINT ( 'NONE',  ( -15.39035576413176187, -80.39644734457957043, 4.330127018922213189 ) ) ;
#15707 = DIRECTION ( 'NONE',  ( -0.1566598588826321747, 0.9876526153536343555, 0.000000000000000000 ) ) ;
#15708 = EDGE_LOOP ( 'NONE', ( #10429, #12798 ) ) ;
#15709 = VERTEX_POINT ( 'NONE', #5821 ) ;
#15710 = AXIS2_PLACEMENT_3D ( 'NONE', #4261, #17554, #6163 ) ;
#15711 = AXIS2_PLACEMENT_3D ( 'NONE', #3970, #16994, #8444 ) ;
#15712 = CARTESIAN_POINT ( 'NONE',  ( -79.24244631363546887, 32.81909429640987952, -24.99999999999999289 ) ) ;
#15713 = ADVANCED_FACE ( 'NONE', ( #6861 ), #8362, .F. ) ;
#15714 = CIRCLE ( 'NONE', #1513, 145.0000000000000284 ) ;
#15715 = DIRECTION ( 'NONE',  ( 0.000000000000000000, 0.000000000000000000, 1.000000000000000000 ) ) ;
#15716 = AXIS2_PLACEMENT_3D ( 'NONE', #6502, #9233, #4680 ) ;
#15717 = CARTESIAN_POINT ( 'NONE',  ( 0.000000000000000000, 0.000000000000000000, 37.00000000000000711 ) ) ;
#15718 = AXIS2_PLACEMENT_3D ( 'NONE', #4902, #10596, #3467 ) ;
#15719 = CIRCLE ( 'NONE', #8463, 1.500000000000000888 ) ;
#15720 = FACE_OUTER_BOUND ( 'NONE', #14417, .T. ) ;
#15721 = CARTESIAN_POINT ( 'NONE',  ( -1.109027851681966492, -20.42569795443330349, -4.330127018922184767 ) ) ;
#15722 = CARTESIAN_POINT ( 'NONE',  ( -19.17624791478365864, -18.22898240811121795, 1.908195823574487804E-14 ) ) ;
#15723 = DIRECTION ( 'NONE',  ( -0.9876526153536336894, -0.1566598588826349503, 0.000000000000000000 ) ) ;
#15724 = CARTESIAN_POINT ( 'NONE',  ( -18.18859529943003750, -18.07232254922858061, -12.99038105676658006 ) ) ;
#15725 = EDGE_LOOP ( 'NONE', ( #3091, #11459 ) ) ;
#15726 = CARTESIAN_POINT ( 'NONE',  ( -34.68921677370541090, -25.75213315644277046, 8.660254037844417496 ) ) ;
#15727 = AXIS2_PLACEMENT_3D ( 'NONE', #1030, #15582, #1114 ) ;
#15728 = FACE_OUTER_BOUND ( 'NONE', #9168, .T. ) ;
#15729 = DIRECTION ( 'NONE',  ( -0.9876526153536336894, -0.1566598588826349503, 0.000000000000000000 ) ) ;
#15730 = ORIENTED_EDGE ( 'NONE', *, *, #1297, .F. ) ;
#15731 = CIRCLE ( 'NONE', #18194, 1.499999999999999556 ) ;
#15732 = CARTESIAN_POINT ( 'NONE',  ( 0.000000000000000000, 0.000000000000000000, 35.00000000000000000 ) ) ;
#15733 = ORIENTED_EDGE ( 'NONE', *, *, #5834, .T. ) ;
#15734 = ORIENTED_EDGE ( 'NONE', *, *, #1444, .T. ) ;
#15735 = AXIS2_PLACEMENT_3D ( 'NONE', #11301, #15496, #2511 ) ;
#15736 = ORIENTED_EDGE ( 'NONE', *, *, #9875, .T. ) ;
#15737 = CYLINDRICAL_SURFACE ( 'NONE', #9366, 1.500000000000001554 ) ;
#15738 = ADVANCED_FACE ( 'NONE', ( #11284 ), #17103, .F. ) ;
#15739 = CIRCLE ( 'NONE', #16671, 1.500000000000000888 ) ;
#15740 = ORIENTED_EDGE ( 'NONE', *, *, #17349, .F. ) ;
#15741 = ORIENTED_EDGE ( 'NONE', *, *, #10008, .T. ) ;
#15742 = CARTESIAN_POINT ( 'NONE',  ( -175.0529311237955596, 56.11526690008648899, 2.500000000000000000 ) ) ;
#15743 = EDGE_LOOP ( 'NONE', ( #13256, #11851, #7177, #1596 ) ) ;
#15744 = ORIENTED_EDGE ( 'NONE', *, *, #516, .T. ) ;
#15745 = CARTESIAN_POINT ( 'NONE',  ( -81.73462711737164454, 33.01666666666666572, 35.00000000000000000 ) ) ;
#15746 = EDGE_CURVE ( 'NONE', #12681, #12642, #7296, .T. ) ;
#15747 = AXIS2_PLACEMENT_3D ( 'NONE', #8243, #14010, #1059 ) ;
#15748 = ORIENTED_EDGE ( 'NONE', *, *, #5128, .F. ) ;
#15749 = CARTESIAN_POINT ( 'NONE',  ( -77.60960976086163043, -0.02410910878642313210, -4.939713573722440465 ) ) ;
#15750 = CIRCLE ( 'NONE', #12087, 1.500000000000001332 ) ;
#15751 = EDGE_LOOP ( 'NONE', ( #4885, #16042, #2322, #4061 ) ) ;
#15752 = VECTOR ( 'NONE', #15084, 1000.000000000000000 ) ;
#15753 = AXIS2_PLACEMENT_3D ( 'NONE', #15479, #16825, #11095 ) ;
#15754 = ORIENTED_EDGE ( 'NONE', *, *, #15922, .T. ) ;
#15755 = DIRECTION ( 'NONE',  ( -0.1566598588826321747, 0.9876526153536343555, 0.000000000000000000 ) ) ;
#15756 = DIRECTION ( 'NONE',  ( -0.1566598588826321192, 0.9876526153536342445, 7.798540720466730171E-17 ) ) ;
#15757 = DIRECTION ( 'NONE',  ( -0.9876526153536336894, -0.1566598588826349503, 0.000000000000000000 ) ) ;
#15758 = CARTESIAN_POINT ( 'NONE',  ( -61.31620237807555895, -87.68113078262194904, -12.99038105676658539 ) ) ;
#15759 = CIRCLE ( 'NONE', #17595, 1.500000000000000888 ) ;
#15760 = CARTESIAN_POINT ( 'NONE',  ( 0.000000000000000000, 0.000000000000000000, 30.00000000000000000 ) ) ;
#15761 = VECTOR ( 'NONE', #641, 1000.000000000000000 ) ;
#15763 = ORIENTED_EDGE ( 'NONE', *, *, #8569, .T. ) ;
#15762 = EDGE_CURVE ( 'NONE', #584, #2390, #12085, .T. ) ;
#15764 = EDGE_LOOP ( 'NONE', ( #12773, #5247 ) ) ;
#15765 = EDGE_LOOP ( 'NONE', ( #14540, #15125 ) ) ;
#15766 = DIRECTION ( 'NONE',  ( -0.9876526153536344665, -0.1566598588826304539, 0.000000000000000000 ) ) ;
#15767 = ADVANCED_FACE ( 'NONE', ( #3464 ), #18021, .F. ) ;
#15768 = EDGE_CURVE ( 'NONE', #15396, #2115, #3621, .T. ) ;
#15769 = ORIENTED_EDGE ( 'NONE', *, *, #8250, .T. ) ;
#15770 = CIRCLE ( 'NONE', #12990, 2.200000000000000178 ) ;
#15771 = FACE_BOUND ( 'NONE', #7114, .T. ) ;
#15772 = EDGE_CURVE ( 'NONE', #11102, #7929, #14247, .T. ) ;
#15773 = AXIS2_PLACEMENT_3D ( 'NONE', #6900, #12469, #13988 ) ;
#15774 = LINE ( 'NONE', #14537, #7855 ) ;
#15775 = LINE ( 'NONE', #8580, #13037 ) ;
#15776 = VECTOR ( 'NONE', #6892, 1000.000000000000000 ) ;
#15777 = CARTESIAN_POINT ( 'NONE',  ( -25.59598991458226536, -19.24727149084832689, 17.32050807568881723 ) ) ;
#15778 = DIRECTION ( 'NONE',  ( 0.000000000000000000, 0.000000000000000000, 1.000000000000000000 ) ) ;
#15779 = APPLICATION_PROTOCOL_DEFINITION ( 'draft international standard', 'automotive_design', 1998, #8228 ) ;
#15780 = AXIS2_PLACEMENT_3D ( 'NONE', #8080, #6496, #2213 ) ;
#15781 = CYLINDRICAL_SURFACE ( 'NONE', #13604, 1.500000000000001554 ) ;
#15782 = DIRECTION ( 'NONE',  ( -0.9876526153536336894, -0.1566598588826349503, 0.000000000000000000 ) ) ;
#15783 = DIRECTION ( 'NONE',  ( -0.1566598588826321192, 0.9876526153536342445, 7.798540720466730171E-17 ) ) ;
#15784 = DIRECTION ( 'NONE',  ( 0.000000000000000000, 0.000000000000000000, -1.000000000000000000 ) ) ;
#15785 = ORIENTED_EDGE ( 'NONE', *, *, #16677, .T. ) ;
#15786 = VERTEX_POINT ( 'NONE', #6449 ) ;
#15787 = FACE_BOUND ( 'NONE', #2614, .T. ) ;
#15788 = DIRECTION ( 'NONE',  ( 0.000000000000000000, 0.000000000000000000, 1.000000000000000000 ) ) ;
#15789 = AXIS2_PLACEMENT_3D ( 'NONE', #84, #18622, #8792 ) ;
#15790 = DIRECTION ( 'NONE',  ( -1.000000000000000000, 0.000000000000000000, 0.000000000000000000 ) ) ;
#15791 = VECTOR ( 'NONE', #547, 1000.000000000000000 ) ;
#15792 = ADVANCED_FACE ( 'NONE', ( #12275 ), #5897, .F. ) ;
#15793 = ORIENTED_EDGE ( 'NONE', *, *, #2364, .F. ) ;
#15794 = DIRECTION ( 'NONE',  ( -0.1566598588826321747, 0.9876526153536343555, 0.000000000000000000 ) ) ;
#15795 = AXIS2_PLACEMENT_3D ( 'NONE', #18530, #17162, #6832 ) ;
#15796 = CARTESIAN_POINT ( 'NONE',  ( -73.49714175923330117, -26.84527464665596597, 17.32050807568882078 ) ) ;
#15797 = DIRECTION ( 'NONE',  ( -0.1566598588826321192, 0.9876526153536342445, 7.798540720466730171E-17 ) ) ;
#15798 = EDGE_CURVE ( 'NONE', #3590, #15891, #748, .T. ) ;
#15799 = AXIS2_PLACEMENT_3D ( 'NONE', #6175, #13249, #16128 ) ;
#15800 = DIRECTION ( 'NONE',  ( -0.9876526153536341335, -0.1566598588826327021, 0.000000000000000000 ) ) ;
#15801 = CARTESIAN_POINT ( 'NONE',  ( -44.56574292724172182, -27.31873174526908699, -8.660254037844380193 ) ) ;
#15802 = FACE_OUTER_BOUND ( 'NONE', #1779, .T. ) ;
#15803 = CARTESIAN_POINT ( 'NONE',  ( -27.57129514528951120, -19.56059120861359091, 1.926565525561698076E-14 ) ) ;
#15804 = APPLICATION_PROTOCOL_DEFINITION ( 'draft international standard', 'automotive_design', 1998, #9191 ) ;
#15805 = ORIENTED_EDGE ( 'NONE', *, *, #526, .F. ) ;
#15806 = AXIS2_PLACEMENT_3D ( 'NONE', #5527, #11280, #15364 ) ;
#15807 = DIRECTION ( 'NONE',  ( -0.1566598588826321192, 0.9876526153536342445, 7.798540720466730171E-17 ) ) ;
#15808 = ORIENTED_EDGE ( 'NONE', *, *, #7729, .T. ) ;
#15809 = CARTESIAN_POINT ( 'NONE',  ( -2.590506774712424853, -20.66068774275724707, -21.65063509461098334 ) ) ;
#15810 = FACE_OUTER_BOUND ( 'NONE', #1241, .T. ) ;
#15811 = CARTESIAN_POINT ( 'NONE',  ( -8.476787456656362352, -79.29982833240114815, -12.99038105676658539 ) ) ;
#15812 = ORIENTED_EDGE ( 'NONE', *, *, #10526, .F. ) ;
#15813 = VECTOR ( 'NONE', #13995, 1000.000000000000000 ) ;
#15814 = CARTESIAN_POINT ( 'NONE',  ( -49.59961335071796640, 35.00051552679457245, -20.00000000000000355 ) ) ;
#15815 = CARTESIAN_POINT ( 'NONE',  ( -77.50990852772314099, -0.1964846621953221517, 5.115456906574511464 ) ) ;
#15816 = ORIENTED_EDGE ( 'NONE', *, *, #5374, .T. ) ;
#15817 = FACE_OUTER_BOUND ( 'NONE', #15275, .T. ) ;
#15818 = ORIENTED_EDGE ( 'NONE', *, *, #2782, .T. ) ;
#15819 = ORIENTED_EDGE ( 'NONE', *, *, #51, .T. ) ;
#15820 = DIRECTION ( 'NONE',  ( -0.1566598588826321192, 0.9876526153536342445, 7.798540720466731404E-17 ) ) ;
#15821 = EDGE_CURVE ( 'NONE', #3794, #7992, #9712, .T. ) ;
#15822 = ORIENTED_EDGE ( 'NONE', *, *, #6884, .F. ) ;
#15823 = CARTESIAN_POINT ( 'NONE',  ( -67.77557938805200877, -31.00023842901093118, -17.32050807568878170 ) ) ;
#15824 = CIRCLE ( 'NONE', #1607, 1.500000000000000888 ) ;
#15825 = DIRECTION ( 'NONE',  ( 0.000000000000000000, 0.000000000000000000, 1.000000000000000000 ) ) ;
#15826 = CARTESIAN_POINT ( 'NONE',  ( -79.05438463828194529, 1.499069270643416107, 2.500000000000000000 ) ) ;
#15827 = DIRECTION ( 'NONE',  ( -0.9876526153536341335, -0.1566598588826327021, 0.000000000000000000 ) ) ;
#15828 = CARTESIAN_POINT ( 'NONE',  ( -6.007655918272284623, -78.90817868519457079, -17.32050807568878525 ) ) ;
#15829 = EDGE_CURVE ( 'NONE', #10552, #8596, #4459, .T. ) ;
#15830 = CARTESIAN_POINT ( 'NONE',  ( -74.62210677719829732, 46.96672731380024146, -2.500000000000000000 ) ) ;
#15831 = CARTESIAN_POINT ( 'NONE',  ( -3.373806069125576901, -15.72242466598909871, 21.65063509461101177 ) ) ;
#15832 = VERTEX_POINT ( 'NONE', #10857 ) ;
#15833 = EDGE_LOOP ( 'NONE', ( #2392, #7128 ) ) ;
#15834 = CARTESIAN_POINT ( 'NONE',  ( -56.37793930130741415, -86.89783148820879433, 4.330127018922213189 ) ) ;
#15835 = AXIS2_PLACEMENT_3D ( 'NONE', #14688, #11823, #9275 ) ;
#15836 = VERTEX_POINT ( 'NONE', #18115 ) ;
#15837 = EDGE_LOOP ( 'NONE', ( #9976, #17839, #6278, #14478 ) ) ;
#15838 = ORIENTED_EDGE ( 'NONE', *, *, #12610, .T. ) ;
#15839 = DIRECTION ( 'NONE',  ( -0.1566598588826321747, 0.9876526153536343555, 0.000000000000000000 ) ) ;
#15840 = FACE_BOUND ( 'NONE', #4369, .T. ) ;
#15841 = CARTESIAN_POINT ( 'NONE',  ( -77.95461635773787634, 0.4738735750096247923, -4.432276680483205666 ) ) ;
#15842 = CIRCLE ( 'NONE', #8591, 3.000000000000000000 ) ;
#15843 = EDGE_CURVE ( 'NONE', #6040, #227, #4979, .T. ) ;
#15844 = DIRECTION ( 'NONE',  ( -0.1566598588826321192, 0.9876526153536342445, 7.798540720466730171E-17 ) ) ;
#15845 = DIRECTION ( 'NONE',  ( -0.9876526153536336894, -0.1566598588826349503, 0.000000000000000000 ) ) ;
#15847 = EDGE_CURVE ( 'NONE', #8275, #4130, #3033, .T. ) ;
#15846 = CARTESIAN_POINT ( 'NONE',  ( -20.65772683781411345, -18.46397219643516507, 1.908195823574487804E-14 ) ) ;
#15848 = LINE ( 'NONE', #14425, #13262 ) ;
#15849 = ORIENTED_EDGE ( 'NONE', *, *, #17409, .T. ) ;
#15850 = VERTEX_POINT ( 'NONE', #15144 ) ;
#15851 = ORIENTED_EDGE ( 'NONE', *, *, #6942, .F. ) ;
#15852 = ORIENTED_EDGE ( 'NONE', *, *, #17465, .T. ) ;
#15853 = CARTESIAN_POINT ( 'NONE',  ( -26.58364252993588650, -19.40393134973095357, -12.99038105676658006 ) ) ;
#15854 = VECTOR ( 'NONE', #7941, 1000.000000000000000 ) ;
#15855 = VERTEX_POINT ( 'NONE', #10683 ) ;
#15856 = FACE_BOUND ( 'NONE', #7033, .T. ) ;
#15857 = CARTESIAN_POINT ( 'NONE',  ( -64.77298653181324539, -88.22944028871114597, -21.65063509461098690 ) ) ;
#15858 = ORIENTED_EDGE ( 'NONE', *, *, #18283, .F. ) ;
#15859 = CARTESIAN_POINT ( 'NONE',  ( -7.528769851480577202, -21.44398703717040888, -21.65063509461098334 ) ) ;
#15860 = CARTESIAN_POINT ( 'NONE',  ( -346.6053245638183853, 10.98772995598034008, 9.951701414186830458E-16 ) ) ;
#15861 = DIRECTION ( 'NONE',  ( 0.000000000000000000, 0.000000000000000000, 1.000000000000000000 ) ) ;
#15862 = DIRECTION ( 'NONE',  ( -0.9876526153536336894, -0.1566598588826349503, 0.000000000000000000 ) ) ;
#15863 = ORIENTED_EDGE ( 'NONE', *, *, #4673, .T. ) ;
#15864 = EDGE_CURVE ( 'NONE', #9857, #5108, #10240, .T. ) ;
#15865 = EDGE_CURVE ( 'NONE', #17419, #9271, #6065, .T. ) ;
#15866 = CARTESIAN_POINT ( 'NONE',  ( -51.27495791377661760, -23.32042782179675200, 12.99038105676661736 ) ) ;
#15867 =( NAMED_UNIT ( * ) PLANE_ANGLE_UNIT ( ) SI_UNIT ( $, .RADIAN. ) );
#15868 = FACE_OUTER_BOUND ( 'NONE', #17429, .T. ) ;
#15869 = EDGE_CURVE ( 'NONE', #7505, #9397, #17597, .T. ) ;
#15870 = CARTESIAN_POINT ( 'NONE',  ( -50.45202360918563045, -85.95787233491302004, 17.32050807568881368 ) ) ;
#15871 = ORIENTED_EDGE ( 'NONE', *, *, #9984, .F. ) ;
#15872 = EDGE_LOOP ( 'NONE', ( #12967, #6332, #1370, #5924 ) ) ;
#15873 = FACE_OUTER_BOUND ( 'NONE', #14602, .T. ) ;
#15874 = ORIENTED_EDGE ( 'NONE', *, *, #14068, .F. ) ;
#15875 = LINE ( 'NONE', #10362, #3524 ) ;
#15876 = FACE_OUTER_BOUND ( 'NONE', #12609, .T. ) ;
#15877 = ORIENTED_EDGE ( 'NONE', *, *, #2193, .F. ) ;
#15878 = DIRECTION ( 'NONE',  ( -0.9876526153536336894, -0.1566598588826349503, 0.000000000000000000 ) ) ;
#15879 = CARTESIAN_POINT ( 'NONE',  ( -128.4427290061107385, 9.376024958400087428, 3.566331213966848601 ) ) ;
#15880 = CIRCLE ( 'NONE', #1373, 1.500000000000000444 ) ;
#15881 = DIRECTION ( 'NONE',  ( 0.1856185419698762329, -0.9826218788918640312, 0.000000000000000000 ) ) ;
#15882 = CARTESIAN_POINT ( 'NONE',  ( -9.464440072009985272, -79.45648819128378193, 8.660254037844412167 ) ) ;
#15883 = SURFACE_SIDE_STYLE ('',( #4223 ) ) ;
#15884 = ORIENTED_EDGE ( 'NONE', *, *, #10112, .F. ) ;
#15885 = ADVANCED_FACE ( 'NONE', ( #11981 ), #2127, .F. ) ;
#15886 = CARTESIAN_POINT ( 'NONE',  ( -6.995308533625909320, -79.06483854407720457, -21.65063509461098690 ) ) ;
#15887 = ORIENTED_EDGE ( 'NONE', *, *, #13198, .F. ) ;
#15888 = LINE ( 'NONE', #13036, #4720 ) ;
#15889 = DIRECTION ( 'NONE',  ( -0.9876526153536336894, -0.1566598588826349503, 0.000000000000000000 ) ) ;
#15890 = CARTESIAN_POINT ( 'NONE',  ( -76.90911978745816668, 1.387778780781445676E-14, 7.500000000000000000 ) ) ;
#15891 = VERTEX_POINT ( 'NONE', #9261 ) ;
#15892 = CARTESIAN_POINT ( 'NONE',  ( -44.85521591397803576, -22.30213873905963951, -12.99038105676658006 ) ) ;
#15894 = ORIENTED_EDGE ( 'NONE', *, *, #9089, .F. ) ;
#15893 = CARTESIAN_POINT ( 'NONE',  ( 8.807133312032172867, -76.55828080195509244, -8.660254037844389075 ) ) ;
#15895 = CIRCLE ( 'NONE', #8016, 1.500000000000000888 ) ;
#15896 = DIRECTION ( 'NONE',  ( -0.1566598588826321192, 0.9876526153536342445, 7.798540720466731404E-17 ) ) ;
#15897 = VERTEX_POINT ( 'NONE', #8735 ) ;
#15898 = ORIENTED_EDGE ( 'NONE', *, *, #5061, .F. ) ;
#15899 = DIRECTION ( 'NONE',  ( -0.1566598588826321192, 0.9876526153536342445, 7.798540720466730171E-17 ) ) ;
#15900 = CARTESIAN_POINT ( 'NONE',  ( 3.231158466157554976, 19.73726462726227382, 30.00000000000000000 ) ) ;
#15901 = DIRECTION ( 'NONE',  ( -0.9876526153536336894, -0.1566598588826349503, 0.000000000000000000 ) ) ;
#15902 = LINE ( 'NONE', #15826, #6700 ) ;
#15903 = CARTESIAN_POINT ( 'NONE',  ( -7.982961148979534016, -79.22149840295983836, 8.660254037844412167 ) ) ;
#15904 = FACE_OUTER_BOUND ( 'NONE', #16954, .T. ) ;
#15905 = FACE_OUTER_BOUND ( 'NONE', #5123, .T. ) ;
#15906 = VECTOR ( 'NONE', #18063, 1000.000000000000114 ) ;
#15907 = VERTEX_POINT ( 'NONE', #13091 ) ;
#15908 = CARTESIAN_POINT ( 'NONE',  ( 2.000000000000000000, 2.449293598294706414E-16, 35.00000000000000000 ) ) ;
#15909 = DIRECTION ( 'NONE',  ( -0.1566598588826321192, 0.9876526153536342445, 7.798540720466730171E-17 ) ) ;
#15910 = CARTESIAN_POINT ( 'NONE',  ( -129.1404785418517918, -2.850701963179328668, 12.74754878398196745 ) ) ;
#15912 = VERTEX_POINT ( 'NONE', #10593 ) ;
#15911 = DIRECTION ( 'NONE',  ( 0.000000000000000000, 0.000000000000000000, 1.000000000000000000 ) ) ;
#15913 = EDGE_CURVE ( 'NONE', #16881, #2, #117, .T. ) ;
#15914 = ORIENTED_EDGE ( 'NONE', *, *, #15155, .T. ) ;
#15915 = ORIENTED_EDGE ( 'NONE', *, *, #15252, .T. ) ;
#15916 = ADVANCED_FACE ( 'NONE', ( #661 ), #12185, .F. ) ;
#15917 = CARTESIAN_POINT ( 'NONE',  ( -31.68662391746665463, -82.98133501614300656, 21.65063509461101532 ) ) ;
#15918 = AXIS2_PLACEMENT_3D ( 'NONE', #7133, #17377, #4360 ) ;
#15919 = ORIENTED_EDGE ( 'NONE', *, *, #990, .F. ) ;
#15920 = VERTEX_POINT ( 'NONE', #2539 ) ;
#15921 = DIRECTION ( 'NONE',  ( -0.1566598588826321747, 0.9876526153536343555, 0.000000000000000000 ) ) ;
#15922 = EDGE_CURVE ( 'NONE', #2300, #7880, #13012, .T. ) ;
#15923 = AXIS2_PLACEMENT_3D ( 'NONE', #14110, #9771, #18534 ) ;
#15924 = CARTESIAN_POINT ( 'NONE',  ( -80.30645961545690170, -27.92535762103354458, 25.00000000000001776 ) ) ;
#15925 = DIRECTION ( 'NONE',  ( -0.1566598588826321192, 0.9876526153536342445, 7.798540720466731404E-17 ) ) ;
#15926 = AXIS2_PLACEMENT_3D ( 'NONE', #986, #7973, #16810 ) ;
#15927 = DIRECTION ( 'NONE',  ( -0.9876526153536336894, -0.1566598588826349503, 0.000000000000000000 ) ) ;
#15928 = VERTEX_POINT ( 'NONE', #5200 ) ;
#15929 = VERTEX_POINT ( 'NONE', #18322 ) ;
#15930 = CARTESIAN_POINT ( 'NONE',  ( -59.67000514428247016, -24.65203662229912851, 21.65063509461101887 ) ) ;
#15931 = DIRECTION ( 'NONE',  ( 0.000000000000000000, 0.000000000000000000, 1.000000000000000000 ) ) ;
#15932 = AXIS2_PLACEMENT_3D ( 'NONE', #2058, #7749, #10484 ) ;
#15933 = CYLINDRICAL_SURFACE ( 'NONE', #15145, 1.500000000000001554 ) ;
#15934 = DIRECTION ( 'NONE',  ( -0.1566598588826321192, 0.9876526153536342445, 7.798540720466730171E-17 ) ) ;
#15935 = FACE_BOUND ( 'NONE', #18235, .T. ) ;
#15936 = DIRECTION ( 'NONE',  ( -0.9998476951563911586, 2.137303368083795934E-18, -0.01745240643728354635 ) ) ;
#15937 = DIRECTION ( 'NONE',  ( -0.1566598588826321192, 0.9876526153536342445, 7.798540720466731404E-17 ) ) ;
#15938 = VERTEX_POINT ( 'NONE', #12561 ) ;
#15939 = ORIENTED_EDGE ( 'NONE', *, *, #2406, .F. ) ;
#15940 = ORIENTED_EDGE ( 'NONE', *, *, #1975, .F. ) ;
#15941 = CARTESIAN_POINT ( 'NONE',  ( -9.504075082187826595, -21.75730675493566579, -12.99038105676658006 ) ) ;
#15942 = AXIS2_PLACEMENT_3D ( 'NONE', #5798, #4532, #14406 ) ;
#15943 = CIRCLE ( 'NONE', #12596, 1.500000000000000444 ) ;
#15944 = EDGE_CURVE ( 'NONE', #1139, #9239, #3660, .T. ) ;
#15945 = ORIENTED_EDGE ( 'NONE', *, *, #12361, .F. ) ;
#15946 = CARTESIAN_POINT ( 'NONE',  ( -76.66445292623467367, -32.41017715895461038, -21.65063509461098334 ) ) ;
#15947 = CARTESIAN_POINT ( 'NONE',  ( -40.61513246582718040, -26.69209230973856251, 21.65063509461101887 ) ) ;
#15948 = ORIENTED_EDGE ( 'NONE', *, *, #9203, .T. ) ;
#15949 = CIRCLE ( 'NONE', #15333, 1.500000000000000000 ) ;
#15950 = EDGE_CURVE ( 'NONE', #18110, #15929, #2735, .T. ) ;
#15951 = AXIS2_PLACEMENT_3D ( 'NONE', #6536, #2068, #10689 ) ;
#15952 = EDGE_CURVE ( 'NONE', #2545, #10257, #15750, .T. ) ;
#15953 = VECTOR ( 'NONE', #4696, 1000.000000000000000 ) ;
#15954 = DIRECTION ( 'NONE',  ( 0.000000000000000000, 1.000000000000000000, 0.000000000000000000 ) ) ;
#15955 = EDGE_LOOP ( 'NONE', ( #7631, #5238 ) ) ;
#15956 = VECTOR ( 'NONE', #13901, 1000.000000000000000 ) ;
#15957 = DIRECTION ( 'NONE',  ( -0.1566598588826321192, 0.9876526153536342445, 7.798540720466730171E-17 ) ) ;
#15958 = CYLINDRICAL_SURFACE ( 'NONE', #6294, 1.500000000000000888 ) ;
#15959 = CARTESIAN_POINT ( 'NONE',  ( -2.000000000000000000, 2.449293598294706414E-16, 35.00000000000000000 ) ) ;
#15960 = DIRECTION ( 'NONE',  ( -0.1566598588826321192, 0.9876526153536342445, 7.798540720466730171E-17 ) ) ;
#15961 = CARTESIAN_POINT ( 'NONE',  ( -29.25712738926042888, -24.89050393258829175, -4.330127018922181215 ) ) ;
#15962 = EDGE_LOOP ( 'NONE', ( #8268, #8923, #5136, #2369 ) ) ;
#15963 = EDGE_LOOP ( 'NONE', ( #14786, #7852 ) ) ;
#15964 = CARTESIAN_POINT ( 'NONE',  ( -47.98289207080156871, -85.56622268770641426, -21.65063509461098690 ) ) ;
#15965 = PRODUCT_DEFINITION_FORMATION_WITH_SPECIFIED_SOURCE ( 'ANY', '', #15287, .NOT_KNOWN. ) ;
#15966 = AXIS2_PLACEMENT_3D ( 'NONE', #1989, #4826, #18137 ) ;
#15967 = CARTESIAN_POINT ( 'NONE',  ( -53.74408945216070776, -23.71207746900332936, 8.660254037844417496 ) ) ;
#15968 = EDGE_CURVE ( 'NONE', #15547, #13951, #4243, .T. ) ;
#15969 = EDGE_CURVE ( 'NONE', #17353, #7282, #8412, .T. ) ;
#15970 = VERTEX_POINT ( 'NONE', #9550 ) ;
#15971 = CARTESIAN_POINT ( 'NONE',  ( -128.1404785157144204, -15.33290121937809403, 2.500000000000000000 ) ) ;
#15972 = AXIS2_PLACEMENT_3D ( 'NONE', #14645, #6116, #4312 ) ;
#15973 = EDGE_CURVE ( 'NONE', #17742, #14531, #4841, .T. ) ;
#15974 = EDGE_CURVE ( 'NONE', #16318, #294, #10876, .T. ) ;
#15975 = DIRECTION ( 'NONE',  ( -0.9826218788918641422, -0.1856185419698762606, 0.000000000000000000 ) ) ;
#15976 = DIRECTION ( 'NONE',  ( -0.000000000000000000, -0.000000000000000000, -1.000000000000000000 ) ) ;
#15977 = CIRCLE ( 'NONE', #6312, 1.500000000000001332 ) ;
#15978 = DIRECTION ( 'NONE',  ( -0.1566598588826321747, 0.9876526153536343555, 0.000000000000000000 ) ) ;
#15979 = DIRECTION ( 'NONE',  ( 1.000000000000000000, 0.000000000000000000, 0.000000000000000000 ) ) ;
#15980 = CARTESIAN_POINT ( 'NONE',  ( -25.76070822534488869, -82.04137586284721806, 17.32050807568881368 ) ) ;
#15981 = DIRECTION ( 'NONE',  ( 1.000000000000000000, 0.000000000000000000, 0.000000000000000000 ) ) ;
#15982 = ORIENTED_EDGE ( 'NONE', *, *, #15974, .T. ) ;
#15983 = CARTESIAN_POINT ( 'NONE',  ( -45.55339554259534651, -27.47539160415172432, -21.65063509461098334 ) ) ;
#15984 = AXIS2_PLACEMENT_3D ( 'NONE', #11806, #95, #8898 ) ;
#15986 = ORIENTED_EDGE ( 'NONE', *, *, #11578, .F. ) ;
#15985 = DIRECTION ( 'NONE',  ( 0.000000000000000000, 0.000000000000000000, 1.000000000000000000 ) ) ;
#15987 = CIRCLE ( 'NONE', #12336, 1.499999999999999556 ) ;
#15988 = CIRCLE ( 'NONE', #4816, 1.500000000000000888 ) ;
#15989 = EDGE_CURVE ( 'NONE', #9368, #17205, #6918, .T. ) ;
#15990 = ORIENTED_EDGE ( 'NONE', *, *, #11786, .F. ) ;
#15991 = EDGE_CURVE ( 'NONE', #6871, #1617, #11485, .T. ) ;
#15992 = AXIS2_PLACEMENT_3D ( 'NONE', #14670, #10679, #1875 ) ;
#15993 = ADVANCED_FACE ( 'NONE', ( #12380 ), #18225, .F. ) ;
#15994 = ADVANCED_FACE ( 'NONE', ( #16784 ), #3745, .F. ) ;
#15995 = DIRECTION ( 'NONE',  ( -0.1566598588826321747, 0.9876526153536343555, 0.000000000000000000 ) ) ;
#15996 = CARTESIAN_POINT ( 'NONE',  ( -51.43967622453926936, -86.11453219379562540, -21.65063509461098690 ) ) ;
#15997 = LINE ( 'NONE', #14398, #15542 ) ;
#15998 = CIRCLE ( 'NONE', #15682, 2.200000000000000622 ) ;
#15999 = DIRECTION ( 'NONE',  ( -0.9876526153536336894, -0.1566598588826349503, 0.000000000000000000 ) ) ;
#16000 = DIRECTION ( 'NONE',  ( 2.735665993912342121E-16, 0.000000000000000000, 1.000000000000000000 ) ) ;
#16001 = AXIS2_PLACEMENT_3D ( 'NONE', #12783, #8343, #8435 ) ;
#16002 = DIRECTION ( 'NONE',  ( -0.000000000000000000, -0.000000000000000000, -1.000000000000000000 ) ) ;
#16003 = AXIS2_PLACEMENT_3D ( 'NONE', #5531, #11089, #11285 ) ;
#16004 = DIRECTION ( 'NONE',  ( 1.000000000000000000, 0.000000000000000000, 0.000000000000000000 ) ) ;
#16005 = FACE_BOUND ( 'NONE', #14551, .T. ) ;
#16006 = DIRECTION ( 'NONE',  ( -0.9876526153536341335, -0.1566598588826327021, 0.000000000000000000 ) ) ;
#16007 = FACE_OUTER_BOUND ( 'NONE', #14961, .T. ) ;
#16009 = ORIENTED_EDGE ( 'NONE', *, *, #4726, .F. ) ;
#16008 = DIRECTION ( 'NONE',  ( -0.1566598588826321747, 0.9876526153536343555, 0.000000000000000000 ) ) ;
#16010 = CLOSED_SHELL ( 'NONE', ( #10661, #8680, #16284, #11153, #3352, #15792, #18649, #9415, #2800, #10343, #6407, #6330, #8353, #873, #10065, #761, #12644, #7661, #2888, #3790, #12919, #13057, #3219, #9788, #9134, #15738, #2313, #12241, #5065, #13390, #12946, #2214, #18677, #17320, #6613, #14682, #16756, #1302, #3475, #2309, #2867, #17376, #13588, #16574, #18702, #12419, #17510, #11662, #9694, #5408, #13885, #10202, #5895, #10318, #7579, #16751, #5565, #9631, #6750, #16995, #12096, #2887, #16528, #18406, #17413, #1630, #2308, #1803, #1910, #809, #18072, #4066, #9357, #18349, #8894, #11994, #12566, #5564, #3951, #6610, #8681, #201, #18159, #5155, #18354, #6671, #18026, #9724, #12496, #10315, #333, #12732, #4085, #2685, #11720, #16225, #6503, #14194, #10048, #7918, #3333, #16813, #10135, #13530, #17895, #16139, #10369, #8315, #5360, #16341, #4704, #7374, #6880, #5029, #1418, #12381, #10911, #1973, #10916, #14124, #18380, #11973, #15617, #3084, #10550, #2334, #4348, #4835, #18550, #15227, #10388, #1273, #16643, #9829, #11828, #17407, #16578, #17519, #1379, #14396, #15618, #5583, #7252, #5162, #12860, #17551, #12021, #4779, #4056, #8998, #1281, #16939, #9744, #18774, #17070, #11942, #8445, #7430, #8698, #4388, #10687, #6444, #6834, #7466, #17920, #18230, #8987, #7380, #13457, #12386, #6167, #754, #7740, #7810, #2665, #9171, #14452, #2103, #14589, #3164, #8093, #6730, #10726, #16976, #414, #9645, #15993, #11235, #6564, #17296, #933, #11091, #4552, #9981, #5000, #15130, #16477, #9092, #1669, #7386, #7618, #7203, #14536, #9718, #9980, #14610, #459, #10765, #15592, #4147, #17264, #600, #12265, #7096, #1604, #6471, #9624, #4499, #3932, #11550, #14311, #10620, #11455, #9326, #10182, #13911, #12995, #6086, #1854, #12932, #8632, #1584, #3403, #7812, #17751, #4204, #18419, #900, #2936, #3740, #106, #3312, #12996, #15767, #3964, #6062, #6147, #12024, #4599, #5900, #3472, #10763, #10527, #579, #14243, #8416, #4146, #15599, #1327, #2642, #7753, #10111, #15713, #12023, #14724, #12192, #13429, #14023, #6853, #17889, #3248, #14479, #11416, #15209, #15454, #6968, #1954, #4831, #14809, #17167, #4999, #14022, #15033, #3810, #13370, #418, #78, #4, #1051, #12800, #14474, #14653, #11177, #1086, #12376, #16164, #12113, #729, #6387, #8392, #5854, #6410, #5966, #9039, #17315, #15280, #1142, #10587, #6991, #14937, #2939, #3455, #16162, #14960, #1653, #6115, #1112, #17395, #1251, #568, #18097, #11881, #4248, #7126, #16908, #15208, #6050, #8776, #13692, #17691, #16705, #4315, #10504, #3746, #5649, #16379, #2661, #13529, #834, #655, #6264, #11436, #15639, #10236, #15994, #3299, #6590, #10269, #15916, #16502, #11938, #1555, #12679, #9407, #2983, #2913, #17975, #14419, #4121, #12739, #2394, #14609, #2543, #14941, #16609, #17392, #5197, #4953, #6504, #6535, #14476, #1557, #8558, #2945, #17759, #4645, #16858, #8657, #8613, #5674, #16121, #9932, #6608, #4408, #2719 ) ) ;
#16011 = ORIENTED_EDGE ( 'NONE', *, *, #7312, .T. ) ;
#16012 = DIRECTION ( 'NONE',  ( -0.9876526153536341335, -0.1566598588826327021, 0.000000000000000000 ) ) ;
#16013 = ORIENTED_EDGE ( 'NONE', *, *, #9593, .F. ) ;
#16014 = VECTOR ( 'NONE', #16423, 1000.000000000000000 ) ;
#16015 = EDGE_LOOP ( 'NONE', ( #3132, #1866, #17560, #7695 ) ) ;
#16017 = ORIENTED_EDGE ( 'NONE', *, *, #1826, .F. ) ;
#16016 = EDGE_CURVE ( 'NONE', #9058, #5802, #14845, .T. ) ;
#16018 = LINE ( 'NONE', #472, #2629 ) ;
#16019 = AXIS2_PLACEMENT_3D ( 'NONE', #3461, #18109, #5075 ) ;
#16020 = AXIS2_PLACEMENT_3D ( 'NONE', #5085, #7950, #749 ) ;
#16021 = FACE_BOUND ( 'NONE', #12983, .T. ) ;
#16022 = ORIENTED_EDGE ( 'NONE', *, *, #2289, .F. ) ;
#16023 = DIRECTION ( 'NONE',  ( 0.000000000000000000, 0.000000000000000000, 1.000000000000000000 ) ) ;
#16024 = ADVANCED_FACE ( 'NONE', ( #162 ), #7292, .T. ) ;
#16025 = AXIS2_PLACEMENT_3D ( 'NONE', #12901, #4193, #8747 ) ;
#16026 = EDGE_CURVE ( 'NONE', #9148, #1188, #18548, .T. ) ;
#16027 = AXIS2_PLACEMENT_3D ( 'NONE', #5317, #11072, #16900 ) ;
#16028 = CARTESIAN_POINT ( 'NONE',  ( -81.73462711737164454, 33.01666666666666572, -35.00000000000000000 ) ) ;
#16029 = ORIENTED_EDGE ( 'NONE', *, *, #2102, .F. ) ;
#16030 = FACE_BOUND ( 'NONE', #4519, .T. ) ;
#16031 = CIRCLE ( 'NONE', #12394, 1.500000000000000888 ) ;
#16032 = VERTEX_POINT ( 'NONE', #15892 ) ;
#16033 = CARTESIAN_POINT ( 'NONE',  ( -39.09401853261888959, -84.15628395776272441, -8.660254037844385522 ) ) ;
#16034 = AXIS2_PLACEMENT_3D ( 'NONE', #11624, #17449, #10217 ) ;
#16035 = CIRCLE ( 'NONE', #7273, 3.000000000000002665 ) ;
#16036 = DIRECTION ( 'NONE',  ( -0.1566598588826321192, 0.9876526153536342445, 7.798540720466731404E-17 ) ) ;
#16037 = CARTESIAN_POINT ( 'NONE',  ( -77.65210554158829837, -32.56683701783724416, 17.32050807568881723 ) ) ;
#16038 = DIRECTION ( 'NONE',  ( -0.1566598588826321192, 0.9876526153536342445, 7.798540720466731404E-17 ) ) ;
#16039 = ORIENTED_EDGE ( 'NONE', *, *, #16522, .F. ) ;
#16040 = ORIENTED_EDGE ( 'NONE', *, *, #4626, .T. ) ;
#16041 = AXIS2_PLACEMENT_3D ( 'NONE', #12743, #4211, #5753 ) ;
#16042 = ORIENTED_EDGE ( 'NONE', *, *, #12362, .F. ) ;
#16043 = CARTESIAN_POINT ( 'NONE',  ( -76.17062661855784711, -32.33184722951329348, -17.32050807568878170 ) ) ;
#16044 = VERTEX_POINT ( 'NONE', #11688 ) ;
#16045 = VECTOR ( 'NONE', #13659, 1000.000000000000000 ) ;
#16046 = CYLINDRICAL_SURFACE ( 'NONE', #3662, 2.200000000000000622 ) ;
#16047 = DIRECTION ( 'NONE',  ( 0.000000000000000000, 0.000000000000000000, 1.000000000000000000 ) ) ;
#16048 = AXIS2_PLACEMENT_3D ( 'NONE', #18669, #2693, #8856 ) ;
#16049 = ORIENTED_EDGE ( 'NONE', *, *, #16965, .F. ) ;
#16050 = AXIS2_PLACEMENT_3D ( 'NONE', #2083, #2154, #13606 ) ;
#16051 = ORIENTED_EDGE ( 'NONE', *, *, #273, .F. ) ;
#16052 = EDGE_CURVE ( 'NONE', #12090, #12954, #17525, .T. ) ;
#16053 = ORIENTED_EDGE ( 'NONE', *, *, #239, .T. ) ;
#16054 = DIRECTION ( 'NONE',  ( -0.1566598588826321192, 0.9876526153536342445, 7.798540720466730171E-17 ) ) ;
#16055 = FACE_BOUND ( 'NONE', #11335, .T. ) ;
#16056 = AXIS2_PLACEMENT_3D ( 'NONE', #9660, #2630, #2454 ) ;
#16057 = DIRECTION ( 'NONE',  ( -0.000000000000000000, -0.000000000000000000, -1.000000000000000000 ) ) ;
#16058 = EDGE_CURVE ( 'NONE', #14768, #18371, #3330, .T. ) ;
#16059 = CARTESIAN_POINT ( 'NONE',  ( -70.24471092643608472, -31.39188807621751209, 21.65063509461101887 ) ) ;
#16061 = CARTESIAN_POINT ( 'NONE',  ( 11.77009115809307715, -76.08830122530719109, 8.660254037844406838 ) ) ;
#16060 = AXIS2_PLACEMENT_3D ( 'NONE', #12810, #18736, #5716 ) ;
#16062 = CARTESIAN_POINT ( 'NONE',  ( -70.29518329010467426, 45.12560182341311332, -5.734307918512490332 ) ) ;
#16063 = AXIS2_PLACEMENT_3D ( 'NONE', #5529, #14240, #11640 ) ;
#16064 = VERTEX_POINT ( 'NONE', #16089 ) ;
#16065 = VERTEX_POINT ( 'NONE', #15700 ) ;
#16066 = DIRECTION ( 'NONE',  ( -0.1566598588826321192, 0.9876526153536342445, 7.798540720466730171E-17 ) ) ;
#16067 = AXIS2_PLACEMENT_3D ( 'NONE', #3541, #6516, #10940 ) ;
#16068 = VERTEX_POINT ( 'NONE', #3089 ) ;
#16069 = EDGE_CURVE ( 'NONE', #11171, #7553, #8784, .T. ) ;
#16070 = CARTESIAN_POINT ( 'NONE',  ( -8.312069145893737243, -16.50572396040226053, -12.99038105676658006 ) ) ;
#16071 = CARTESIAN_POINT ( 'NONE',  ( -45.51376053241747144, -85.17457304049985112, 17.32050807568881368 ) ) ;
#16072 = EDGE_LOOP ( 'NONE', ( #18175, #1698 ) ) ;
#16073 = FACE_OUTER_BOUND ( 'NONE', #1368, .T. ) ;
#16074 = AXIS2_PLACEMENT_3D ( 'NONE', #1851, #431, #10279 ) ;
#16075 = AXIS2_PLACEMENT_3D ( 'NONE', #14003, #2625, #1234 ) ;
#16076 = CARTESIAN_POINT ( 'NONE',  ( -53.74408945216070776, -23.71207746900332936, 8.660254037844417496 ) ) ;
#16077 = DIRECTION ( 'NONE',  ( 1.000000000000000000, 0.000000000000000000, -0.000000000000000000 ) ) ;
#16078 = CARTESIAN_POINT ( 'NONE',  ( -66.08974714408108753, -25.67032570503621614, -12.99038105676658006 ) ) ;
#16079 =( NAMED_UNIT ( * ) SI_UNIT ( $, .STERADIAN. ) SOLID_ANGLE_UNIT ( ) );
#16080 = AXIS2_PLACEMENT_3D ( 'NONE', #16855, #15409, #12359 ) ;
#16081 = EDGE_CURVE ( 'NONE', #5805, #9632, #2989, .T. ) ;
#16082 = CARTESIAN_POINT ( 'NONE',  ( -58.84707083969148300, -87.28948113541537168, 1.424741226644455312E-14 ) ) ;
#16083 = CARTESIAN_POINT ( 'NONE',  ( 55.85952145814821534, 6.938893903907228378E-15, -30.00000000000000000 ) ) ;
#16084 = AXIS2_PLACEMENT_3D ( 'NONE', #14579, #1683, #5950 ) ;
#16085 = CARTESIAN_POINT ( 'NONE',  ( -81.87192997736541145, 3.395211045985502274, 2.500000000000000000 ) ) ;
#16086 = CARTESIAN_POINT ( 'NONE',  ( 3.868870235264020963, -77.34158009636824715, 17.32050807568880657 ) ) ;
#16087 = VERTEX_POINT ( 'NONE', #14469 ) ;
#16088 = ORIENTED_EDGE ( 'NONE', *, *, #6709, .T. ) ;
#16089 = CARTESIAN_POINT ( 'NONE',  ( -61.84966369593023927, -30.06027927571514624, -12.99038105676658006 ) ) ;
#16090 = VERTEX_POINT ( 'NONE', #7196 ) ;
#16091 = EDGE_CURVE ( 'NONE', #8605, #17569, #3642, .T. ) ;
#16092 = CIRCLE ( 'NONE', #1893, 1.500000000000001332 ) ;
#16093 = DIRECTION ( 'NONE',  ( -0.1566598588826321192, 0.9876526153536342445, 7.798540720466730171E-17 ) ) ;
#16094 = EDGE_CURVE ( 'NONE', #15303, #18000, #2147, .T. ) ;
#16095 = EDGE_LOOP ( 'NONE', ( #6541, #12688 ) ) ;
#16096 = CIRCLE ( 'NONE', #18567, 1.500000000000000888 ) ;
#16097 = ORIENTED_EDGE ( 'NONE', *, *, #1083, .T. ) ;
#16098 = CARTESIAN_POINT ( 'NONE',  ( -23.12685837619818940, -18.85562184364173532, -21.65063509461098334 ) ) ;
#16099 = CIRCLE ( 'NONE', #4878, 1.499999999999999556 ) ;
#16100 = DIRECTION ( 'NONE',  ( 1.000000000000000000, 0.000000000000000000, 0.000000000000000000 ) ) ;
#16101 = CARTESIAN_POINT ( 'NONE',  ( 0.000000000000000000, 0.000000000000000000, 30.00000000000000000 ) ) ;
#16102 = EDGE_CURVE ( 'NONE', #8498, #9656, #2726, .T. ) ;
#16103 = CARTESIAN_POINT ( 'NONE',  ( -0.4108482230646692823, -15.25244508934120802, 21.65063509461101177 ) ) ;
#16104 = DIRECTION ( 'NONE',  ( -0.1566598588826321192, 0.9876526153536342445, 7.798540720466730171E-17 ) ) ;
#16105 = CARTESIAN_POINT ( 'NONE',  ( -38.14600092744311155, -26.30044266253198160, -17.32050807568878170 ) ) ;
#16106 = CIRCLE ( 'NONE', #11245, 1.500000000000001332 ) ;
#16107 = CYLINDRICAL_SURFACE ( 'NONE', #17545, 145.0000000000000284 ) ;
#16108 = EDGE_LOOP ( 'NONE', ( #1061, #14186, #4681, #12202 ) ) ;
#16109 = CARTESIAN_POINT ( 'NONE',  ( -70.24471092643608472, -31.39188807621751209, 12.99038105676661736 ) ) ;
#16110 = CONICAL_SURFACE ( 'NONE', #3365, 15.74754878398195856, 0.01745329251994333364 ) ;
#16111 = EDGE_CURVE ( 'NONE', #356, #14582, #8803, .T. ) ;
#16112 = DIRECTION ( 'NONE',  ( -0.9876526153536336894, -0.1566598588826350336, 0.000000000000000000 ) ) ;
#16113 = CARTESIAN_POINT ( 'NONE',  ( 5.481473465377021625, 12.88229205725314763, 25.00000000000000000 ) ) ;
#16114 = EDGE_CURVE ( 'NONE', #3127, #2423, #11502, .T. ) ;
#16116 = ORIENTED_EDGE ( 'NONE', *, *, #7027, .T. ) ;
#16115 = DIRECTION ( 'NONE',  ( -0.1566598588826321192, 0.9876526153536342445, 7.798540720466730171E-17 ) ) ;
#16117 = EDGE_CURVE ( 'NONE', #4398, #3127, #14297, .T. ) ;
#16118 =( GEOMETRIC_REPRESENTATION_CONTEXT ( 3 ) GLOBAL_UNCERTAINTY_ASSIGNED_CONTEXT ( ( #9278 ) ) GLOBAL_UNIT_ASSIGNED_CONTEXT ( ( #681, #8628, #975 ) ) REPRESENTATION_CONTEXT ( 'NONE', 'WORKASPACE' ) );
#16119 = ORIENTED_EDGE ( 'NONE', *, *, #6436, .T. ) ;
#16120 = CYLINDRICAL_SURFACE ( 'NONE', #5041, 1.500000000000001554 ) ;
#16121 = ADVANCED_FACE ( 'NONE', ( #7111 ), #18697, .F. ) ;
#16122 = ORIENTED_EDGE ( 'NONE', *, *, #5511, .F. ) ;
#16123 = EDGE_CURVE ( 'NONE', #2946, #17353, #16681, .T. ) ;
#16124 = ORIENTED_EDGE ( 'NONE', *, *, #1411, .T. ) ;
#16125 = ORIENTED_EDGE ( 'NONE', *, *, #4137, .F. ) ;
#16126 = CARTESIAN_POINT ( 'NONE',  ( -25.80034323552273179, -24.34219442649909126, 4.330127018922217630 ) ) ;
#16127 = AXIS2_PLACEMENT_3D ( 'NONE', #7942, #13610, #7844 ) ;
#16128 = DIRECTION ( 'NONE',  ( -0.9876526153536341335, -0.1566598588826327021, 0.000000000000000000 ) ) ;
#16129 = CARTESIAN_POINT ( 'NONE',  ( -52.26261052913025651, -23.47708768067938223, 1.926565525561698076E-14 ) ) ;
#16130 = UNCERTAINTY_MEASURE_WITH_UNIT (LENGTH_MEASURE( 1.000000000000000082E-05 ), #9497, 'distance_accuracy_value', 'NONE');
#16131 = VERTEX_POINT ( 'NONE', #15814 ) ;
#16132 = EDGE_CURVE ( 'NONE', #10693, #8732, #4852, .T. ) ;
#16133 = ORIENTED_EDGE ( 'NONE', *, *, #2864, .F. ) ;
#16134 = COLOUR_RGB ( '', 0.72549020, 0.75294118, 0.79215686) ;
#16135 = CARTESIAN_POINT ( 'NONE',  ( -40.41077914488671041, -21.59716937408778037, 1.214306433183764966E-14 ) ) ;
#16136 = CARTESIAN_POINT ( 'NONE',  ( 6.338001773648100468, -76.94993044916168401, 12.99038105676660493 ) ) ;
#16137 = EDGE_CURVE ( 'NONE', #6687, #17343, #34, .T. ) ;
#16138 = VERTEX_POINT ( 'NONE', #77 ) ;
#16139 = ADVANCED_FACE ( 'NONE', ( #5861 ), #4961, .F. ) ;
#16140 = EDGE_LOOP ( 'NONE', ( #80, #17529 ) ) ;
#16141 = ORIENTED_EDGE ( 'NONE', *, *, #10496, .F. ) ;
#16142 = ORIENTED_EDGE ( 'NONE', *, *, #4063, .F. ) ;
#16143 = FACE_BOUND ( 'NONE', #14644, .T. ) ;
#16144 = CARTESIAN_POINT ( 'NONE',  ( -66.08974714408108753, -25.67032570503621969, -4.330127018922180326 ) ) ;
#16145 = ORIENTED_EDGE ( 'NONE', *, *, #2192, .F. ) ;
#16146 = AXIS2_PLACEMENT_3D ( 'NONE', #5611, #10136, #17187 ) ;
#16147 = CYLINDRICAL_SURFACE ( 'NONE', #2712, 1.500000000000001554 ) ;
#16148 = ORIENTED_EDGE ( 'NONE', *, *, #12671, .F. ) ;
#16149 = ORIENTED_EDGE ( 'NONE', *, *, #9491, .F. ) ;
#16150 = CARTESIAN_POINT ( 'NONE',  ( -25.80034323552273179, -24.34219442649909126, -12.99038105676658006 ) ) ;
#16151 = DIRECTION ( 'NONE',  ( 0.000000000000000000, 0.000000000000000000, 1.000000000000000000 ) ) ;
#16152 = DIRECTION ( 'NONE',  ( 0.000000000000000000, 0.000000000000000000, 1.000000000000000000 ) ) ;
#16153 = DIRECTION ( 'NONE',  ( 2.671473304378624222E-16, 0.000000000000000000, 1.000000000000000000 ) ) ;
#16154 = DIRECTION ( 'NONE',  ( 1.000000000000000000, 0.000000000000000000, -2.671473304378624222E-16 ) ) ;
#16155 = ORIENTED_EDGE ( 'NONE', *, *, #15973, .T. ) ;
#16156 = EDGE_LOOP ( 'NONE', ( #17073, #6072 ) ) ;
#16157 = AXIS2_PLACEMENT_3D ( 'NONE', #17646, #16383, #16188 ) ;
#16158 = FACE_BOUND ( 'NONE', #2266, .T. ) ;
#16159 = DIRECTION ( 'NONE',  ( -6.505213034913026604E-17, -0.000000000000000000, 1.000000000000000000 ) ) ;
#16160 = EDGE_LOOP ( 'NONE', ( #984, #7908, #7528, #14367 ) ) ;
#16161 = CARTESIAN_POINT ( 'NONE',  ( -25.26688191766805858, -81.96304593340589406, 21.65063509461101532 ) ) ;
#16162 = ADVANCED_FACE ( 'NONE', ( #14932 ), #10568, .F. ) ;
#16163 = DIRECTION ( 'NONE',  ( 1.000000000000000000, 0.000000000000000000, 0.000000000000000000 ) ) ;
#16164 = ADVANCED_FACE ( 'NONE', ( #11785 ), #17719, .F. ) ;
#16165 = VERTEX_POINT ( 'NONE', #17632 ) ;
#16166 = DIRECTION ( 'NONE',  ( -0.1566598588826321192, 0.9876526153536342445, 7.798540720466731404E-17 ) ) ;
#16167 = LINE ( 'NONE', #4945, #1788 ) ;
#16168 = EDGE_CURVE ( 'NONE', #10248, #1545, #12062, .T. ) ;
#16169 = FACE_BOUND ( 'NONE', #2631, .T. ) ;
#16170 = LINE ( 'NONE', #14650, #16998 ) ;
#16171 = DIRECTION ( 'NONE',  ( -0.9876526153536336894, -0.1566598588826349503, 0.000000000000000000 ) ) ;
#16172 = DIRECTION ( 'NONE',  ( -0.9876526153536336894, -0.1566598588826349503, 0.000000000000000000 ) ) ;
#16173 =( LENGTH_UNIT ( ) NAMED_UNIT ( * ) SI_UNIT ( .MILLI., .METRE. ) );
#16174 = ORIENTED_EDGE ( 'NONE', *, *, #15772, .T. ) ;
#16175 = CARTESIAN_POINT ( 'NONE',  ( 55.85952145814821534, 6.938893903907228378E-15, 35.00000000000000000 ) ) ;
#16176 = DIRECTION ( 'NONE',  ( -0.1566598588826321192, 0.9876526153536342445, 7.798540720466730171E-17 ) ) ;
#16177 = DIRECTION ( 'NONE',  ( -0.000000000000000000, -0.000000000000000000, 1.000000000000000000 ) ) ;
#16178 = CARTESIAN_POINT ( 'NONE',  ( 2.881217619910392269, -77.49823995525089515, -4.330127018922189208 ) ) ;
#16179 = ORIENTED_EDGE ( 'NONE', *, *, #519, .F. ) ;
#16180 = ORIENTED_EDGE ( 'NONE', *, *, #17229, .F. ) ;
#16181 = CARTESIAN_POINT ( 'NONE',  ( -43.08426400421126345, -27.08374195694514341, -17.32050807568878170 ) ) ;
#16182 = ORIENTED_EDGE ( 'NONE', *, *, #13745, .T. ) ;
#16183 = ORIENTED_EDGE ( 'NONE', *, *, #4867, .T. ) ;
#16184 = EDGE_CURVE ( 'NONE', #18301, #10629, #16693, .T. ) ;
#16185 = AXIS2_PLACEMENT_3D ( 'NONE', #13169, #8918, #6380 ) ;
#16186 = DIRECTION ( 'NONE',  ( -0.1566598588826321192, 0.9876526153536342445, 7.798540720466730171E-17 ) ) ;
#16187 = CYLINDRICAL_SURFACE ( 'NONE', #3953, 1.500000000000001554 ) ;
#16188 = DIRECTION ( 'NONE',  ( -0.9876526153536336894, -0.1566598588826349503, 0.000000000000000000 ) ) ;
#16189 = ORIENTED_EDGE ( 'NONE', *, *, #4019, .T. ) ;
#16190 = FACE_OUTER_BOUND ( 'NONE', #17918, .T. ) ;
#16191 = CARTESIAN_POINT ( 'NONE',  ( -25.26688191766805858, -81.96304593340589406, 12.99038105676661203 ) ) ;
#16192 = ADVANCED_FACE ( 'NONE', ( #4605, #13686 ), #13406, .F. ) ;
#16193 = CARTESIAN_POINT ( 'NONE',  ( -20.82244514857674389, -81.25807656843406335, 1.424741226644455312E-14 ) ) ;
#16194 = EDGE_LOOP ( 'NONE', ( #14166, #2148, #11651, #11729 ) ) ;
#16195 = CARTESIAN_POINT ( 'NONE',  ( -5.059638313096497697, -21.05233738996382797, 8.660254037844412167 ) ) ;
#16196 = CARTESIAN_POINT ( 'NONE',  ( -6.057127952975085021E-15, 2.200000000000023270, -130.3485206753969976 ) ) ;
#16197 = DIRECTION ( 'NONE',  ( -0.9876526153536341335, -0.1566598588826327576, 0.000000000000000000 ) ) ;
#16198 = AXIS2_PLACEMENT_3D ( 'NONE', #12935, #7549, #15889 ) ;
#16199 = ORIENTED_EDGE ( 'NONE', *, *, #3692, .T. ) ;
#16200 = ORIENTED_EDGE ( 'NONE', *, *, #4288, .T. ) ;
#16201 = CARTESIAN_POINT ( 'NONE',  ( -61.15148406731293562, -24.88702641062306142, -4.330127018922180326 ) ) ;
#16202 = ORIENTED_EDGE ( 'NONE', *, *, #990, .T. ) ;
#16203 = ORIENTED_EDGE ( 'NONE', *, *, #11571, .F. ) ;
#16204 = DIRECTION ( 'NONE',  ( -0.1566598588826321747, 0.9876526153536343555, 0.000000000000000000 ) ) ;
#16205 = CARTESIAN_POINT ( 'NONE',  ( 3.000000000000004441, 3.673940397442064798E-16, -20.00000000000000355 ) ) ;
#16206 = EDGE_LOOP ( 'NONE', ( #8078, #4451, #2575, #15816, #16524 ) ) ;
#16207 = EDGE_CURVE ( 'NONE', #592, #1113, #7735, .T. ) ;
#16208 = EDGE_CURVE ( 'NONE', #1459, #8907, #951, .T. ) ;
#16209 = DIRECTION ( 'NONE',  ( -0.1566598588826321747, 0.9876526153536343555, 0.000000000000000000 ) ) ;
#16210 = CIRCLE ( 'NONE', #8937, 1.500000000000000444 ) ;
#16211 = CARTESIAN_POINT ( 'NONE',  ( -48.80582637539256297, -22.92877817459016754, 1.908195823574487804E-14 ) ) ;
#16212 = EDGE_CURVE ( 'NONE', #14096, #15836, #13633, .T. ) ;
#16213 = CARTESIAN_POINT ( 'NONE',  ( -54.73174206751432536, -23.86873732788596669, 12.99038105676661736 ) ) ;
#16214 = CARTESIAN_POINT ( 'NONE',  ( -12.46703292824872733, -22.22728633158356359, 12.99038105676661381 ) ) ;
#16215 = VERTEX_POINT ( 'NONE', #11960 ) ;
#16216 = VERTEX_POINT ( 'NONE', #3444 ) ;
#16217 = CIRCLE ( 'NONE', #9254, 1.500000000000000000 ) ;
#16218 = DIRECTION ( 'NONE',  ( -0.9876526153536341335, -0.1566598588826327021, 0.000000000000000000 ) ) ;
#16219 = LINE ( 'NONE', #11837, #10836 ) ;
#16220 = AXIS2_PLACEMENT_3D ( 'NONE', #870, #1255, #6745 ) ;
#16221 = EDGE_LOOP ( 'NONE', ( #13133, #3133 ) ) ;
#16222 = ORIENTED_EDGE ( 'NONE', *, *, #9903, .T. ) ;
#16223 = EDGE_LOOP ( 'NONE', ( #1208, #18015, #1136, #17480 ) ) ;
#16224 = CARTESIAN_POINT ( 'NONE',  ( -24.81269062016911064, -24.18553456761645393, 8.660254037844417496 ) ) ;
#16225 = ADVANCED_FACE ( 'NONE', ( #3361 ), #6329, .F. ) ;
#16226 = ORIENTED_EDGE ( 'NONE', *, *, #15472, .F. ) ;
#16227 = FACE_BOUND ( 'NONE', #247, .T. ) ;
#16228 = EDGE_CURVE ( 'NONE', #5860, #14458, #5796, .T. ) ;
#16229 = DIRECTION ( 'NONE',  ( 0.000000000000000000, 0.000000000000000000, -1.000000000000000000 ) ) ;
#16230 = EDGE_CURVE ( 'NONE', #12256, #14223, #1269, .T. ) ;
#16231 = EDGE_LOOP ( 'NONE', ( #466, #11611, #9385, #2366 ) ) ;
#16232 = FILL_AREA_STYLE ('',( #6393 ) ) ;
#16233 = ORIENTED_EDGE ( 'NONE', *, *, #5918, .T. ) ;
#16234 = CIRCLE ( 'NONE', #15629, 1.500000000000000888 ) ;
#16235 = ORIENTED_EDGE ( 'NONE', *, *, #13917, .F. ) ;
#16236 = LINE ( 'NONE', #14905, #12696 ) ;
#16237 = DIRECTION ( 'NONE',  ( -0.9876526153536341335, -0.1566598588826327021, 0.000000000000000000 ) ) ;
#16238 = FACE_OUTER_BOUND ( 'NONE', #1027, .T. ) ;
#16239 = LINE ( 'NONE', #9138, #9246 ) ;
#16240 = DIRECTION ( 'NONE',  ( 8.693966348389027220E-17, -1.991237296706374949E-16, 1.000000000000000000 ) ) ;
#16241 = ORIENTED_EDGE ( 'NONE', *, *, #5639, .T. ) ;
#16242 = VERTEX_POINT ( 'NONE', #7831 ) ;
#16243 = LINE ( 'NONE', #12141, #17527 ) ;
#16244 = DIRECTION ( 'NONE',  ( -0.1566598588826321192, 0.9876526153536342445, 7.798540720466731404E-17 ) ) ;
#16245 = ORIENTED_EDGE ( 'NONE', *, *, #7816, .F. ) ;
#16246 = EDGE_LOOP ( 'NONE', ( #12564, #9470, #10338, #10910 ) ) ;
#16247 = CARTESIAN_POINT ( 'NONE',  ( 2.881217619910392269, -77.49823995525089515, 4.330127018922209636 ) ) ;
#16248 = ORIENTED_EDGE ( 'NONE', *, *, #5784, .T. ) ;
#16249 = AXIS2_PLACEMENT_3D ( 'NONE', #13691, #5185, #10946 ) ;
#16250 = AXIS2_PLACEMENT_3D ( 'NONE', #16178, #13317, #18086 ) ;
#16251 = CARTESIAN_POINT ( 'NONE',  ( -77.44775222064782838, -27.47191408218649400, 21.65063509461101887 ) ) ;
#16252 = AXIS2_PLACEMENT_3D ( 'NONE', #6434, #6338, #18007 ) ;
#16253 = DIRECTION ( 'NONE',  ( -0.9868632313631133801, 0.1615579233078772436, -0.000000000000000000 ) ) ;
#16254 = CARTESIAN_POINT ( 'NONE',  ( -53.94844277310117064, -28.80700040465408662, 12.99038105676661736 ) ) ;
#16255 =( NAMED_UNIT ( * ) SI_UNIT ( $, .STERADIAN. ) SOLID_ANGLE_UNIT ( ) );
#16256 = EDGE_CURVE ( 'NONE', #2654, #13974, #5163, .T. ) ;
#16257 = ORIENTED_EDGE ( 'NONE', *, *, #14864, .T. ) ;
#16258 = EDGE_CURVE ( 'NONE', #3229, #13151, #10740, .T. ) ;
#16259 = CARTESIAN_POINT ( 'NONE',  ( -14.23798483801550674, -17.44568311369805969, -8.660254037844380193 ) ) ;
#16260 = CIRCLE ( 'NONE', #1447, 1.500000000000000444 ) ;
#16261 = CARTESIAN_POINT ( 'NONE',  ( -28.26947477390680774, -24.73384407370567217, -8.660254037844380193 ) ) ;
#16262 = STYLED_ITEM ( 'NONE', ( #1944 ), #14079 ) ;
#16263 = AXIS2_PLACEMENT_3D ( 'NONE', #10271, #7270, #4402 ) ;
#16264 = CARTESIAN_POINT ( 'NONE',  ( -36.62488699423479943, -83.76463431055617548, 4.330127018922213189 ) ) ;
#16265 = ORIENTED_EDGE ( 'NONE', *, *, #1465, .T. ) ;
#16266 = DIRECTION ( 'NONE',  ( -0.9876526153536336894, -0.1566598588826349503, 0.000000000000000000 ) ) ;
#16267 = ORIENTED_EDGE ( 'NONE', *, *, #7350, .T. ) ;
#16268 = AXIS2_PLACEMENT_3D ( 'NONE', #6820, #7112, #5672 ) ;
#16269 = DIRECTION ( 'NONE',  ( -0.9876526153536341335, -0.1566598588826327021, 0.000000000000000000 ) ) ;
#16270 = ORIENTED_EDGE ( 'NONE', *, *, #18305, .F. ) ;
#16271 = DIRECTION ( 'NONE',  ( -0.1566598588826321192, 0.9876526153536342445, 7.798540720466730171E-17 ) ) ;
#16272 = AXIS2_PLACEMENT_3D ( 'NONE', #16827, #9510, #9600 ) ;
#16273 = EDGE_LOOP ( 'NONE', ( #14994, #7405 ) ) ;
#16274 = DIRECTION ( 'NONE',  ( -0.2333333333333339477, -0.9723968097209879646, 0.000000000000000000 ) ) ;
#16275 = FACE_OUTER_BOUND ( 'NONE', #12306, .T. ) ;
#16276 = DIRECTION ( 'NONE',  ( -0.1566598588826321192, 0.9876526153536342445, 7.798540720466731404E-17 ) ) ;
#16277 = AXIS2_PLACEMENT_3D ( 'NONE', #18536, #4052, #1160 ) ;
#16278 = PLANE ( 'NONE',  #9339 ) ;
#16279 = VERTEX_POINT ( 'NONE', #16547 ) ;
#16280 = CARTESIAN_POINT ( 'NONE',  ( 1.360103686702108128, -20.03404830722672259, -8.660254037844383745 ) ) ;
#16281 = CIRCLE ( 'NONE', #18756, 1.499999999999997335 ) ;
#16282 = DIRECTION ( 'NONE',  ( -0.1566598588826321192, 0.9876526153536342445, 7.798540720466730171E-17 ) ) ;
#16283 = ORIENTED_EDGE ( 'NONE', *, *, #14126, .T. ) ;
#16284 = ADVANCED_FACE ( 'NONE', ( #3538 ), #9335, .F. ) ;
#16286 = EDGE_LOOP ( 'NONE', ( #2725, #6867, #2785, #10379 ) ) ;
#16285 = CYLINDRICAL_SURFACE ( 'NONE', #9669, 2.000000000000000000 ) ;
#16287 = CIRCLE ( 'NONE', #9018, 1.500000000000000444 ) ;
#16288 = ORIENTED_EDGE ( 'NONE', *, *, #2555, .T. ) ;
#16289 = DIRECTION ( 'NONE',  ( -0.1566598588826321192, 0.9876526153536342445, 7.798540720466731404E-17 ) ) ;
#16290 = EDGE_LOOP ( 'NONE', ( #17848, #18412, #15020, #11297 ) ) ;
#16291 = EDGE_CURVE ( 'NONE', #411, #18427, #16377, .T. ) ;
#16292 = VERTEX_POINT ( 'NONE', #2232 ) ;
#16293 = ORIENTED_EDGE ( 'NONE', *, *, #10855, .T. ) ;
#16294 = DIRECTION ( 'NONE',  ( 0.000000000000000000, 0.000000000000000000, 1.000000000000000000 ) ) ;
#16295 = ORIENTED_EDGE ( 'NONE', *, *, #3055, .F. ) ;
#16296 = AXIS2_PLACEMENT_3D ( 'NONE', #8284, #18066, #5143 ) ;
#16297 = DIRECTION ( 'NONE',  ( -0.1566598588826321192, 0.9876526153536342445, 7.798540720466730171E-17 ) ) ;
#16298 = ORIENTED_EDGE ( 'NONE', *, *, #10643, .T. ) ;
#16299 = CIRCLE ( 'NONE', #7231, 2.500000000000002220 ) ;
#16300 = DIRECTION ( 'NONE',  ( -0.1566598588826321192, 0.9876526153536342445, 7.798540720466730171E-17 ) ) ;
#16301 = DIRECTION ( 'NONE',  ( 0.000000000000000000, 0.000000000000000000, 1.000000000000000000 ) ) ;
#16302 = DIRECTION ( 'NONE',  ( -0.1566598588826321192, 0.9876526153536342445, 7.798540720466730171E-17 ) ) ;
#16303 = PRESENTATION_LAYER_ASSIGNMENT (  '', '', ( #5726 ) ) ;
#16304 = CARTESIAN_POINT ( 'NONE',  ( -129.1237011781999797, -14.52069893526757127, -5.132545408516867802 ) ) ;
#16305 = CARTESIAN_POINT ( 'NONE',  ( -9.504075082187823043, -21.75730675493566579, 21.65063509461101177 ) ) ;
#16306 = DIRECTION ( 'NONE',  ( -0.1566598588826321192, 0.9876526153536342445, 7.798540720466731404E-17 ) ) ;
#16307 = CARTESIAN_POINT ( 'NONE',  ( -84.20693962813486166, 32.64562644091790844, -30.00000000000000355 ) ) ;
#16308 = ORIENTED_EDGE ( 'NONE', *, *, #14134, .T. ) ;
#16309 = VECTOR ( 'NONE', #14035, 1000.000000000000000 ) ;
#16310 = CARTESIAN_POINT ( 'NONE',  ( -2.000000000000000000, 0.000000000000000000, 30.00000000000000000 ) ) ;
#16311 = EDGE_LOOP ( 'NONE', ( #6478, #7979 ) ) ;
#16312 = EDGE_CURVE ( 'NONE', #4310, #1682, #18300, .T. ) ;
#16313 = CARTESIAN_POINT ( 'NONE',  ( -28.06512145296634486, -19.63892113805490780, 21.65063509461101887 ) ) ;
#16314 = CIRCLE ( 'NONE', #17540, 1.500000000000000888 ) ;
#16315 = CIRCLE ( 'NONE', #10554, 1.500000000000000000 ) ;
#16316 = CARTESIAN_POINT ( 'NONE',  ( -7.982961148979534016, -79.22149840295983836, -17.32050807568878525 ) ) ;
#16317 = AXIS2_PLACEMENT_3D ( 'NONE', #11467, #17301, #198 ) ;
#16318 = VERTEX_POINT ( 'NONE', #2421 ) ;
#16319 = EDGE_CURVE ( 'NONE', #10598, #1633, #9727, .T. ) ;
#16320 = ORIENTED_EDGE ( 'NONE', *, *, #3430, .T. ) ;
#16321 = EDGE_LOOP ( 'NONE', ( #14622, #9781, #18742, #14713 ) ) ;
#16322 = ORIENTED_EDGE ( 'NONE', *, *, #2552, .F. ) ;
#16323 = CARTESIAN_POINT ( 'NONE',  ( -68.55887868246516348, -26.06197535224280415, 8.660254037844417496 ) ) ;
#16324 = FACE_BOUND ( 'NONE', #6799, .T. ) ;
#16325 = VECTOR ( 'NONE', #9268, 1000.000000000000000 ) ;
#16326 = CYLINDRICAL_SURFACE ( 'NONE', #7061, 1.500000000000001554 ) ;
#16327 = AXIS2_PLACEMENT_3D ( 'NONE', #9007, #6382, #12011 ) ;
#16328 = ORIENTED_EDGE ( 'NONE', *, *, #15060, .F. ) ;
#16329 = AXIS2_PLACEMENT_3D ( 'NONE', #8684, #7372, #11603 ) ;
#16330 = AXIS2_PLACEMENT_3D ( 'NONE', #16362, #1753, #7541 ) ;
#16331 = CIRCLE ( 'NONE', #1516, 1.500000000000000888 ) ;
#16332 = AXIS2_PLACEMENT_3D ( 'NONE', #11010, #9614, #2407 ) ;
#16333 = VERTEX_POINT ( 'NONE', #6797 ) ;
#16334 = CARTESIAN_POINT ( 'NONE',  ( -45.55339554259533230, -27.47539160415171722, -4.330127018922181215 ) ) ;
#16335 = LINE ( 'NONE', #9133, #2438 ) ;
#16336 = CYLINDRICAL_SURFACE ( 'NONE', #15131, 1.500000000000000666 ) ;
#16337 = DIRECTION ( 'NONE',  ( 0.000000000000000000, 0.000000000000000000, 1.000000000000000000 ) ) ;
#16338 = CIRCLE ( 'NONE', #13304, 1.500000000000000444 ) ;
#16339 = DIRECTION ( 'NONE',  ( -0.1566598588826321192, 0.9876526153536342445, 7.798540720466730171E-17 ) ) ;
#16340 = ADVANCED_BREP_SHAPE_REPRESENTATION ( '', ( #15126, #18772 ), #17189 ) ;
#16341 = ADVANCED_FACE ( 'NONE', ( #13874 ), #16944, .F. ) ;
#16342 = FACE_OUTER_BOUND ( 'NONE', #2843, .T. ) ;
#16343 = ORIENTED_EDGE ( 'NONE', *, *, #12985, .T. ) ;
#16344 = EDGE_LOOP ( 'NONE', ( #13548, #12467 ) ) ;
#16345 = CARTESIAN_POINT ( 'NONE',  ( -23.12685837619818940, -18.85562184364174243, -4.330127018922180326 ) ) ;
#16346 = EDGE_CURVE ( 'NONE', #6192, #8055, #16390, .T. ) ;
#16347 = AXIS2_PLACEMENT_3D ( 'NONE', #5622, #3984, #7145 ) ;
#16348 = EDGE_LOOP ( 'NONE', ( #6601, #16848, #7657, #3772 ) ) ;
#16349 = DIRECTION ( 'NONE',  ( -0.1566598588826321192, 0.9876526153536342445, 7.798540720466730171E-17 ) ) ;
#16350 = EDGE_CURVE ( 'NONE', #10352, #14662, #6714, .T. ) ;
#16351 = DIRECTION ( 'NONE',  ( -0.1566598588826321192, 0.9876526153536342445, 7.798540720466731404E-17 ) ) ;
#16352 = AXIS2_PLACEMENT_3D ( 'NONE', #2035, #3438, #13585 ) ;
#16353 = EDGE_CURVE ( 'NONE', #11687, #9583, #6708, .T. ) ;
#16354 = ORIENTED_EDGE ( 'NONE', *, *, #1331, .T. ) ;
#16355 = AXIS2_PLACEMENT_3D ( 'NONE', #711, #7809, #13571 ) ;
#16356 = ORIENTED_EDGE ( 'NONE', *, *, #3117, .F. ) ;
#16357 = DIRECTION ( 'NONE',  ( 0.000000000000000000, 0.000000000000000000, 1.000000000000000000 ) ) ;
#16358 = FACE_BOUND ( 'NONE', #8915, .T. ) ;
#16359 = VECTOR ( 'NONE', #16093, 1000.000000000000000 ) ;
#16360 = DIRECTION ( 'NONE',  ( -0.9876526153536341335, -0.1566598588826327021, 0.000000000000000000 ) ) ;
#16361 = AXIS2_PLACEMENT_3D ( 'NONE', #5082, #4802, #16680 ) ;
#16362 = CARTESIAN_POINT ( 'NONE',  ( -14.23798483801550674, -17.44568311369805613, -17.32050807568878170 ) ) ;
#16363 = CIRCLE ( 'NONE', #8190, 1.500000000000000888 ) ;
#16364 = CARTESIAN_POINT ( 'NONE',  ( -57.89905323451570496, -29.43363984018461466, 17.32050807568881723 ) ) ;
#16365 = AXIS2_PLACEMENT_3D ( 'NONE', #6641, #16414, #10610 ) ;
#16366 = DIRECTION ( 'NONE',  ( 0.000000000000000000, 0.000000000000000000, 1.000000000000000000 ) ) ;
#16367 = DIRECTION ( 'NONE',  ( -0.1566598588826321192, 0.9876526153536342445, 7.798540720466730171E-17 ) ) ;
#16368 = EDGE_CURVE ( 'NONE', #10552, #12139, #13340, .T. ) ;
#16369 = ORIENTED_EDGE ( 'NONE', *, *, #16026, .T. ) ;
#16370 = EDGE_LOOP ( 'NONE', ( #3612, #8111, #2932, #12353 ) ) ;
#16371 = DIRECTION ( 'NONE',  ( -1.000000000000000000, 0.000000000000000000, -0.000000000000000000 ) ) ;
#16372 = VERTEX_POINT ( 'NONE', #8010 ) ;
#16373 = EDGE_LOOP ( 'NONE', ( #4784, #11964, #9891, #3969 ) ) ;
#16374 = AXIS2_PLACEMENT_3D ( 'NONE', #5047, #6415, #15013 ) ;
#16375 = EDGE_LOOP ( 'NONE', ( #18700, #11047, #2501, #13380 ) ) ;
#16376 = VERTEX_POINT ( 'NONE', #5460 ) ;
#16377 = CIRCLE ( 'NONE', #17917, 150.0000000000000284 ) ;
#16378 = EDGE_LOOP ( 'NONE', ( #9252, #232, #6784, #12490 ) ) ;
#16379 = ADVANCED_FACE ( 'NONE', ( #821 ), #18491, .F. ) ;
#16380 = DIRECTION ( 'NONE',  ( -0.1566598588826321747, 0.9876526153536343555, 0.000000000000000000 ) ) ;
#16381 = VECTOR ( 'NONE', #11313, 1000.000000000000000 ) ;
#16382 = CARTESIAN_POINT ( 'NONE',  ( -79.23462711737164454, 33.01666666666666572, -35.00000000000000000 ) ) ;
#16383 = DIRECTION ( 'NONE',  ( -0.1566598588826321192, 0.9876526153536342445, 7.798540720466730171E-17 ) ) ;
#16384 = ORIENTED_EDGE ( 'NONE', *, *, #712, .T. ) ;
#16385 = CARTESIAN_POINT ( 'NONE',  ( -14.44233815895597672, -22.54060604934882051, 12.99038105676661381 ) ) ;
#16386 = FILL_AREA_STYLE ('',( #551 ) ) ;
#16387 = VERTEX_POINT ( 'NONE', #3915 ) ;
#16388 = AXIS2_PLACEMENT_3D ( 'NONE', #7818, #15108, #13580 ) ;
#16389 = DIRECTION ( 'NONE',  ( -0.9876526153536336894, -0.1566598588826349503, 0.000000000000000000 ) ) ;
#16390 = CIRCLE ( 'NONE', #8213, 1.500000000000000444 ) ;
#16391 = DIRECTION ( 'NONE',  ( -0.9876526153536341335, -0.1566598588826327576, 0.000000000000000000 ) ) ;
#16392 = FACE_BOUND ( 'NONE', #6297, .T. ) ;
#16393 = CARTESIAN_POINT ( 'NONE',  ( -69.99999999999998579, -45.00000000000000711, 25.00000000000000000 ) ) ;
#16394 = AXIS2_PLACEMENT_3D ( 'NONE', #1009, #11100, #6781 ) ;
#16395 = DIRECTION ( 'NONE',  ( -0.1566598588826321747, 0.9876526153536343555, 0.000000000000000000 ) ) ;
#16397 = ORIENTED_EDGE ( 'NONE', *, *, #15392, .T. ) ;
#16396 = DIRECTION ( 'NONE',  ( -1.000000000000000000, 0.000000000000000000, 0.000000000000000000 ) ) ;
#16398 = AXIS2_PLACEMENT_3D ( 'NONE', #16247, #9228, #11868 ) ;
#16399 = DIRECTION ( 'NONE',  ( -0.9876526153536336894, -0.1566598588826349503, 0.000000000000000000 ) ) ;
#16400 = ORIENTED_EDGE ( 'NONE', *, *, #12246, .F. ) ;
#16401 = EDGE_LOOP ( 'NONE', ( #18108, #18160, #6328, #5535 ) ) ;
#16402 = EDGE_CURVE ( 'NONE', #4043, #7608, #1031, .T. ) ;
#16403 = VECTOR ( 'NONE', #12396, 1000.000000000000000 ) ;
#16404 = ORIENTED_EDGE ( 'NONE', *, *, #10746, .F. ) ;
#16405 = AXIS2_PLACEMENT_3D ( 'NONE', #4932, #16512, #17777 ) ;
#16406 = DIRECTION ( 'NONE',  ( 0.000000000000000000, 0.000000000000000000, 1.000000000000000000 ) ) ;
#16407 = EDGE_CURVE ( 'NONE', #8789, #10862, #9114, .T. ) ;
#16408 = EDGE_CURVE ( 'NONE', #3308, #15217, #2604, .T. ) ;
#16409 = CARTESIAN_POINT ( 'NONE',  ( -76.90911978745816668, 1.387778780781445676E-14, 25.00000000000000000 ) ) ;
#16410 = VERTEX_POINT ( 'NONE', #8389 ) ;
#16411 = AXIS2_PLACEMENT_3D ( 'NONE', #3179, #10206, #13141 ) ;
#16412 = EDGE_CURVE ( 'NONE', #8596, #17674, #12428, .T. ) ;
#16413 = CARTESIAN_POINT ( 'NONE',  ( -3.578159390066044665, -20.81734760163988440, 8.660254037844412167 ) ) ;
#16414 = DIRECTION ( 'NONE',  ( -0.1566598588826321747, 0.9876526153536343555, 0.000000000000000000 ) ) ;
#16415 = FACE_OUTER_BOUND ( 'NONE', #16803, .T. ) ;
#16416 = DIRECTION ( 'NONE',  ( -0.1566598588826321192, 0.9876526153536342445, 7.798540720466730171E-17 ) ) ;
#16417 = CYLINDRICAL_SURFACE ( 'NONE', #10810, 1.500000000000001554 ) ;
#16418 = ORIENTED_EDGE ( 'NONE', *, *, #3610, .F. ) ;
#16419 = AXIS2_PLACEMENT_3D ( 'NONE', #3397, #12406, #15350 ) ;
#16420 = DIRECTION ( 'NONE',  ( -0.1566598588826321192, 0.9876526153536342445, 7.798540720466730171E-17 ) ) ;
#16421 = ORIENTED_EDGE ( 'NONE', *, *, #15048, .T. ) ;
#16422 = CARTESIAN_POINT ( 'NONE',  ( -19.87442754340095519, -23.40223527320329922, 1.869203119972154228E-14 ) ) ;
#16423 = DIRECTION ( 'NONE',  ( -0.1566598588826321192, 0.9876526153536342445, 7.798540720466730171E-17 ) ) ;
#16424 = CIRCLE ( 'NONE', #1597, 2.500000000000002220 ) ;
#16425 = ORIENTED_EDGE ( 'NONE', *, *, #13328, .T. ) ;
#16426 = ORIENTED_EDGE ( 'NONE', *, *, #9153, .F. ) ;
#16427 = ORIENTED_EDGE ( 'NONE', *, *, #11389, .F. ) ;
#16428 = CARTESIAN_POINT ( 'NONE',  ( -31.72625892764450484, -25.28215357979487266, 1.887572821959364500E-14 ) ) ;
#16429 = ORIENTED_EDGE ( 'NONE', *, *, #8697, .T. ) ;
#16430 = FACE_BOUND ( 'NONE', #13727, .T. ) ;
#16431 = VECTOR ( 'NONE', #12871, 1000.000000000000000 ) ;
#16432 = EDGE_CURVE ( 'NONE', #13974, #6246, #967, .T. ) ;
#16433 = DIRECTION ( 'NONE',  ( -0.1566598588826321192, 0.9876526153536342445, 7.798540720466730171E-17 ) ) ;
#16434 = ORIENTED_EDGE ( 'NONE', *, *, #14732, .F. ) ;
#16435 = CIRCLE ( 'NONE', #12482, 3.000000000000000888 ) ;
#16436 = ORIENTED_EDGE ( 'NONE', *, *, #9066, .F. ) ;
#16437 = EDGE_CURVE ( 'NONE', #14246, #3468, #10903, .T. ) ;
#16438 = DIRECTION ( 'NONE',  ( -0.1566598588826321747, 0.9876526153536343555, 0.000000000000000000 ) ) ;
#16439 = LINE ( 'NONE', #3420, #9388 ) ;
#16440 = FACE_OUTER_BOUND ( 'NONE', #3189, .T. ) ;
#16441 = DIRECTION ( 'NONE',  ( -1.000000000000000000, 0.000000000000000000, 0.000000000000000000 ) ) ;
#16442 = CARTESIAN_POINT ( 'NONE',  ( -2.000000000000000000, 0.000000000000000000, 30.00000000000000000 ) ) ;
#16443 = DIRECTION ( 'NONE',  ( 0.000000000000000000, 0.000000000000000000, 1.000000000000000000 ) ) ;
#16444 = VERTEX_POINT ( 'NONE', #9813 ) ;
#16445 = ORIENTED_EDGE ( 'NONE', *, *, #16916, .T. ) ;
#16446 = FACE_OUTER_BOUND ( 'NONE', #14910, .T. ) ;
#16447 = CARTESIAN_POINT ( 'NONE',  ( -30.04042668367358360, -19.95224085582017892, 21.65063509461101887 ) ) ;
#16448 = AXIS2_PLACEMENT_3D ( 'NONE', #11552, #18645, #7055 ) ;
#16449 = EDGE_LOOP ( 'NONE', ( #1033, #7993 ) ) ;
#16450 = LINE ( 'NONE', #17792, #18252 ) ;
#16451 = EDGE_CURVE ( 'NONE', #10528, #1792, #5179, .T. ) ;
#16452 = CARTESIAN_POINT ( 'NONE',  ( -14.23798483801550674, -17.44568311369805969, -8.660254037844380193 ) ) ;
#16453 = EDGE_CURVE ( 'NONE', #5727, #6686, #15583, .T. ) ;
#16454 = CARTESIAN_POINT ( 'NONE',  ( -46.33669483700847280, -22.53712852738359018, 4.330127018922218518 ) ) ;
#16455 = CARTESIAN_POINT ( 'NONE',  ( -309.1404785418517918, -2.850701963179328668, 9.951701414186818625E-16 ) ) ;
#16456 =( NAMED_UNIT ( * ) PLANE_ANGLE_UNIT ( ) SI_UNIT ( $, .RADIAN. ) );
#16457 = EDGE_CURVE ( 'NONE', #3665, #13180, #4271, .T. ) ;
#16458 = ORIENTED_EDGE ( 'NONE', *, *, #4968, .T. ) ;
#16459 = VECTOR ( 'NONE', #11528, 1000.000000000000000 ) ;
#16460 = DIRECTION ( 'NONE',  ( 0.000000000000000000, 0.000000000000000000, 1.000000000000000000 ) ) ;
#16461 = CARTESIAN_POINT ( 'NONE',  ( -70.04035760549561473, -26.29696514056674417, -8.660254037844380193 ) ) ;
#16462 = PLANE ( 'NONE',  #1679 ) ;
#16463 = ORIENTED_EDGE ( 'NONE', *, *, #12771, .F. ) ;
#16464 = ORIENTED_EDGE ( 'NONE', *, *, #14687, .F. ) ;
#16465 = DIRECTION ( 'NONE',  ( -0.1566598588826321192, 0.9876526153536342445, 7.798540720466730171E-17 ) ) ;
#16466 = ORIENTED_EDGE ( 'NONE', *, *, #15162, .T. ) ;
#16467 = ORIENTED_EDGE ( 'NONE', *, *, #7027, .F. ) ;
#16468 = ORIENTED_EDGE ( 'NONE', *, *, #8355, .T. ) ;
#16469 = DIRECTION ( 'NONE',  ( -0.1566598588826321747, 0.9876526153536343555, 0.000000000000000000 ) ) ;
#16470 = EDGE_LOOP ( 'NONE', ( #6499, #3783 ) ) ;
#16471 = DIRECTION ( 'NONE',  ( -0.1566598588826321192, 0.9876526153536342445, 7.798540720466730171E-17 ) ) ;
#16472 = EDGE_CURVE ( 'NONE', #8310, #626, #13556, .T. ) ;
#16473 = FACE_OUTER_BOUND ( 'NONE', #4291, .T. ) ;
#16474 = CARTESIAN_POINT ( 'NONE',  ( 0.000000000000000000, 0.000000000000000000, 35.00000000000000000 ) ) ;
#16475 = ORIENTED_EDGE ( 'NONE', *, *, #11572, .T. ) ;
#16476 = DIRECTION ( 'NONE',  ( 1.000000000000000000, 0.000000000000000000, 0.000000000000000000 ) ) ;
#16477 = ADVANCED_FACE ( 'NONE', ( #11493 ), #1211, .T. ) ;
#16478 = FACE_OUTER_BOUND ( 'NONE', #823, .T. ) ;
#16479 = CARTESIAN_POINT ( 'NONE',  ( -21.64537945316773460, -18.62063205531779531, -12.99038105676658006 ) ) ;
#16480 = CARTESIAN_POINT ( 'NONE',  ( -34.15575545585073058, -83.37298466334958391, 1.424741226644455312E-14 ) ) ;
#16481 = DIRECTION ( 'NONE',  ( -0.1566598588826321192, 0.9876526153536342445, 7.798540720466730171E-17 ) ) ;
#16482 = FACE_OUTER_BOUND ( 'NONE', #17499, .T. ) ;
#16483 = ORIENTED_EDGE ( 'NONE', *, *, #9464, .T. ) ;
#16484 = DIRECTION ( 'NONE',  ( -0.1566598588826321192, 0.9876526153536342445, 7.798540720466730171E-17 ) ) ;
#16485 = VERTEX_POINT ( 'NONE', #8592 ) ;
#16486 = EDGE_LOOP ( 'NONE', ( #2676, #17294, #14570, #15769 ) ) ;
#16487 = EDGE_LOOP ( 'NONE', ( #9025, #7132 ) ) ;
#16488 = FACE_OUTER_BOUND ( 'NONE', #13284, .T. ) ;
#16489 = DIRECTION ( 'NONE',  ( -0.000000000000000000, -0.000000000000000000, -1.000000000000000000 ) ) ;
#16490 = ORIENTED_EDGE ( 'NONE', *, *, #15672, .T. ) ;
#16491 = DIRECTION ( 'NONE',  ( -0.1566598588826321192, 0.9876526153536342445, 7.798540720466731404E-17 ) ) ;
#16492 = PRODUCT_DEFINITION_CONTEXT ( 'detailed design', #10387, 'design' ) ;
#16493 = CARTESIAN_POINT ( 'NONE',  ( -57.69469991357524208, -24.33871690453384318, -21.65063509461098334 ) ) ;
#16494 = VECTOR ( 'NONE', #14189, 1000.000000000000000 ) ;
#16495 = DIRECTION ( 'NONE',  ( -0.1566598588826321747, 0.9876526153536343555, 0.000000000000000000 ) ) ;
#16496 = DIRECTION ( 'NONE',  ( 0.000000000000000000, 0.000000000000000000, -1.000000000000000000 ) ) ;
#16497 = EDGE_CURVE ( 'NONE', #2286, #11293, #11590, .T. ) ;
#16498 = ADVANCED_FACE ( 'NONE', ( #18592 ), #10268, .F. ) ;
#16499 = SURFACE_SIDE_STYLE ('',( #16595 ) ) ;
#16500 = LINE ( 'NONE', #12114, #14377 ) ;
#16501 = PLANE ( 'NONE',  #1213 ) ;
#16502 = ADVANCED_FACE ( 'NONE', ( #57 ), #13018, .F. ) ;
#16503 = ORIENTED_EDGE ( 'NONE', *, *, #13562, .T. ) ;
#16504 = EDGE_LOOP ( 'NONE', ( #1353, #13515, #8631, #881 ) ) ;
#16505 = ORIENTED_EDGE ( 'NONE', *, *, #2850, .F. ) ;
#16506 = VERTEX_POINT ( 'NONE', #14552 ) ;
#16507 = CARTESIAN_POINT ( 'NONE',  ( -53.74408945216072198, -23.71207746900331870, -17.32050807568878170 ) ) ;
#16508 = VERTEX_POINT ( 'NONE', #11308 ) ;
#16509 = CIRCLE ( 'NONE', #1665, 1.500000000000001332 ) ;
#16510 = FACE_BOUND ( 'NONE', #5540, .T. ) ;
#16511 = CYLINDRICAL_SURFACE ( 'NONE', #5227, 1.500000000000000888 ) ;
#16512 = DIRECTION ( 'NONE',  ( -0.1566598588826321747, 0.9876526153536343555, 0.000000000000000000 ) ) ;
#16513 = DIRECTION ( 'NONE',  ( -0.1566598588826321192, 0.9876526153536342445, 7.798540720466730171E-17 ) ) ;
#16514 = CIRCLE ( 'NONE', #17134, 13.99999999999999822 ) ;
#16515 = DIRECTION ( 'NONE',  ( 0.000000000000000000, 0.000000000000000000, 1.000000000000000000 ) ) ;
#16516 = DIRECTION ( 'NONE',  ( -0.1566598588826321192, 0.9876526153536342445, 7.798540720466731404E-17 ) ) ;
#16517 = PLANE ( 'NONE',  #11050 ) ;
#16518 = DIRECTION ( 'NONE',  ( -0.1566598588826321192, 0.9876526153536342445, 7.798540720466730171E-17 ) ) ;
#16519 = ORIENTED_EDGE ( 'NONE', *, *, #12594, .T. ) ;
#16520 = EDGE_LOOP ( 'NONE', ( #18094, #17007, #14861, #7698 ) ) ;
#16521 = FACE_OUTER_BOUND ( 'NONE', #11915, .T. ) ;
#16522 = EDGE_CURVE ( 'NONE', #9759, #12329, #12953, .T. ) ;
#16523 = DIRECTION ( 'NONE',  ( -0.9876526153536336894, -0.1566598588826349503, 0.000000000000000000 ) ) ;
#16524 = ORIENTED_EDGE ( 'NONE', *, *, #11519, .T. ) ;
#16525 = AXIS2_PLACEMENT_3D ( 'NONE', #6006, #4394, #8754 ) ;
#16526 = ORIENTED_EDGE ( 'NONE', *, *, #4314, .F. ) ;
#16527 = CARTESIAN_POINT ( 'NONE',  ( 2.447859171744382056, -14.79900155049411659, 30.00000000000000000 ) ) ;
#16528 = ADVANCED_FACE ( 'NONE', ( #5746 ), #3071, .F. ) ;
#16529 = CARTESIAN_POINT ( 'NONE',  ( -0.4108482230646692823, -15.25244508934120802, 12.99038105676661026 ) ) ;
#16530 = CARTESIAN_POINT ( 'NONE',  ( -173.4288256112363342, 56.32277901880416238, -2.821239268406350753 ) ) ;
#16531 = ORIENTED_EDGE ( 'NONE', *, *, #2244, .F. ) ;
#16532 = CIRCLE ( 'NONE', #1997, 1.500000000000000888 ) ;
#16533 = EDGE_CURVE ( 'NONE', #15443, #4155, #2806, .T. ) ;
#16534 = DIRECTION ( 'NONE',  ( -0.9876526153536336894, -0.1566598588826349503, 0.000000000000000000 ) ) ;
#16535 = DIRECTION ( 'NONE',  ( 0.000000000000000000, 0.000000000000000000, 1.000000000000000000 ) ) ;
#16536 = CARTESIAN_POINT ( 'NONE',  ( -74.19532138785061193, -32.01852751174804013, -17.32050807568878170 ) ) ;
#16537 = DIRECTION ( 'NONE',  ( 0.000000000000000000, 0.000000000000000000, 1.000000000000000000 ) ) ;
#16538 = ORIENTED_EDGE ( 'NONE', *, *, #14752, .F. ) ;
#16539 = AXIS2_PLACEMENT_3D ( 'NONE', #2370, #18261, #13933 ) ;
#16540 = FACE_OUTER_BOUND ( 'NONE', #8264, .T. ) ;
#16541 = DIRECTION ( 'NONE',  ( 1.000000000000000000, 0.000000000000000000, 0.000000000000000000 ) ) ;
#16542 = LINE ( 'NONE', #817, #3292 ) ;
#16543 = EDGE_CURVE ( 'NONE', #11671, #794, #10167, .T. ) ;
#16544 = DIRECTION ( 'NONE',  ( -0.1566598588826321192, 0.9876526153536342445, 7.798540720466731404E-17 ) ) ;
#16545 = ORIENTED_EDGE ( 'NONE', *, *, #11619, .T. ) ;
#16546 = ORIENTED_EDGE ( 'NONE', *, *, #4969, .F. ) ;
#16547 = CARTESIAN_POINT ( 'NONE',  ( -18.18859529943003750, -18.07232254922858417, 4.330127018922218518 ) ) ;
#16548 = EDGE_CURVE ( 'NONE', #3382, #17212, #13858, .T. ) ;
#16549 = AXIS2_PLACEMENT_3D ( 'NONE', #12557, #2246, #12377 ) ;
#16550 = ORIENTED_EDGE ( 'NONE', *, *, #9408, .T. ) ;
#16551 = ORIENTED_EDGE ( 'NONE', *, *, #3098, .F. ) ;
#16552 = DIRECTION ( 'NONE',  ( -0.1566598588826321747, 0.9876526153536343555, 0.000000000000000000 ) ) ;
#16553 = B_SPLINE_CURVE_WITH_KNOTS ( 'NONE', 3,
 ( #4308, #10081, #2872, #14547, #8669, #1475, #16062, #1734, #7263, #5840, #3067, #8859, #6007, #11756, #4582, #2113, #6403, #10645, #14908, #17697 ),
 .UNSPECIFIED., .F., .F.,
 ( 4, 2, 2, 2, 2, 2, 2, 2, 2, 4 ),
 ( 0.000000000000000000, 0.0009785969257606898751, 0.001467895388641035463, 0.001957193851521381485, 0.002935790777282072661, 0.003914387703042764705, 0.004892984628803457615, 0.005871581554564148792, 0.006850178480324841702, 0.007828775406085534613 ),
 .UNSPECIFIED. ) ;
#16554 = ORIENTED_EDGE ( 'NONE', *, *, #7642, .F. ) ;
#16555 = VERTEX_POINT ( 'NONE', #12834 ) ;
#16556 = ORIENTED_EDGE ( 'NONE', *, *, #16453, .F. ) ;
#16557 = EDGE_CURVE ( 'NONE', #16292, #15023, #4494, .T. ) ;
#16558 = CIRCLE ( 'NONE', #4743, 12.74754878398196567 ) ;
#16559 = CIRCLE ( 'NONE', #17171, 1.500000000000000888 ) ;
#16560 = EDGE_CURVE ( 'NONE', #9583, #13845, #10818, .T. ) ;
#16561 = LINE ( 'NONE', #2151, #10863 ) ;
#16562 = DIRECTION ( 'NONE',  ( -0.1566598588826321192, 0.9876526153536342445, 7.798540720466730171E-17 ) ) ;
#16563 = CARTESIAN_POINT ( 'NONE',  ( -59.83472345504510770, -87.44614099429799126, -4.330127018922185655 ) ) ;
#16564 = CARTESIAN_POINT ( 'NONE',  ( -27.28182215855319015, -24.57718421482303484, -21.65063509461098334 ) ) ;
#16565 = VECTOR ( 'NONE', #12536, 1000.000000000000000 ) ;
#16566 = CARTESIAN_POINT ( 'NONE',  ( -28.26947477390680774, -24.73384407370567217, 1.869203119972154228E-14 ) ) ;
#16567 = CIRCLE ( 'NONE', #8391, 1.499999999999999556 ) ;
#16568 = CARTESIAN_POINT ( 'NONE',  ( -8.516422466834198346, -21.60064689605303911, -17.32050807568878170 ) ) ;
#16569 = DIRECTION ( 'NONE',  ( -0.1566598588826321192, 0.9876526153536342445, 7.798540720466731404E-17 ) ) ;
#16570 = VECTOR ( 'NONE', #17885, 1000.000000000000000 ) ;
#16571 = DIRECTION ( 'NONE',  ( 0.000000000000000000, 0.000000000000000000, 1.000000000000000000 ) ) ;
#16572 = VERTEX_POINT ( 'NONE', #10086 ) ;
#16573 = CARTESIAN_POINT ( 'NONE',  ( -36.46016868347218320, -20.97052993855727010, -4.330127018922180326 ) ) ;
#16574 = ADVANCED_FACE ( 'NONE', ( #15873 ), #2875, .F. ) ;
#16575 = EDGE_LOOP ( 'NONE', ( #11425, #15120 ) ) ;
#16576 = ADVANCED_FACE ( 'NONE', ( #14451, #8495, #11666 ), #17501, .F. ) ;
#16577 = DIRECTION ( 'NONE',  ( 1.000000000000000000, 0.000000000000000000, 0.000000000000000000 ) ) ;
#16578 = ADVANCED_FACE ( 'NONE', ( #18676 ), #9993, .F. ) ;
#16579 =( GEOMETRIC_REPRESENTATION_CONTEXT ( 3 ) GLOBAL_UNCERTAINTY_ASSIGNED_CONTEXT ( ( #10232 ) ) GLOBAL_UNIT_ASSIGNED_CONTEXT ( ( #18607, #1589, #70 ) ) REPRESENTATION_CONTEXT ( 'NONE', 'WORKASPACE' ) );
#16580 = VERTEX_POINT ( 'NONE', #7632 ) ;
#16581 = VECTOR ( 'NONE', #9315, 1000.000000000000000 ) ;
#16582 = EDGE_LOOP ( 'NONE', ( #389, #10935 ) ) ;
#16583 = ORIENTED_EDGE ( 'NONE', *, *, #14923, .F. ) ;
#16584 = DIRECTION ( 'NONE',  ( -0.1566598588826321192, 0.9876526153536342445, 7.798540720466730171E-17 ) ) ;
#16585 = DIRECTION ( 'NONE',  ( -0.1566598588826321192, 0.9876526153536342445, 7.798540720466731404E-17 ) ) ;
#16586 = VERTEX_POINT ( 'NONE', #3239 ) ;
#16587 = LINE ( 'NONE', #1984, #17298 ) ;
#16588 = CARTESIAN_POINT ( 'NONE',  ( -129.1404785418517918, -2.850701963179328668, -13.78215425775057490 ) ) ;
#16589 = CARTESIAN_POINT ( 'NONE',  ( -128.5664531142840872, -15.03275830328938945, -3.724467847532855647 ) ) ;
#16590 = FACE_OUTER_BOUND ( 'NONE', #12409, .T. ) ;
#16591 = ORIENTED_EDGE ( 'NONE', *, *, #4673, .F. ) ;
#16592 = FACE_OUTER_BOUND ( 'NONE', #6800, .T. ) ;
#16593 = EDGE_LOOP ( 'NONE', ( #18783, #3110 ) ) ;
#16594 = CIRCLE ( 'NONE', #18760, 1.500000000000000888 ) ;
#16595 = SURFACE_STYLE_FILL_AREA ( #13538 ) ;
#16596 = DIRECTION ( 'NONE',  ( 1.000000000000000000, 0.000000000000000000, 0.000000000000000000 ) ) ;
#16597 = CARTESIAN_POINT ( 'NONE',  ( -126.1404785418517918, -15.29729532696464922, 2.500000000000000000 ) ) ;
#16598 = EDGE_CURVE ( 'NONE', #16165, #18092, #13248, .T. ) ;
#16599 = LINE ( 'NONE', #16807, #603 ) ;
#16600 = AXIS2_PLACEMENT_3D ( 'NONE', #16480, #7751, #18224 ) ;
#16601 = VECTOR ( 'NONE', #17412, 1000.000000000000000 ) ;
#16602 = VERTEX_POINT ( 'NONE', #6114 ) ;
#16603 = ORIENTED_EDGE ( 'NONE', *, *, #1505, .T. ) ;
#16604 = ORIENTED_EDGE ( 'NONE', *, *, #5088, .F. ) ;
#16605 = LINE ( 'NONE', #12416, #4421 ) ;
#16606 = AXIS2_PLACEMENT_3D ( 'NONE', #18246, #9568, #1900 ) ;
#16607 = CIRCLE ( 'NONE', #6935, 1.500000000000000888 ) ;
#16608 = FACE_BOUND ( 'NONE', #14797, .T. ) ;
#16609 = ADVANCED_FACE ( 'NONE', ( #16521 ), #13389, .F. ) ;
#16610 = EDGE_CURVE ( 'NONE', #56, #14073, #14485, .T. ) ;
#16611 = EDGE_LOOP ( 'NONE', ( #2964, #14694, #5524, #6168 ) ) ;
#16612 = DIRECTION ( 'NONE',  ( -0.1566598588826321192, 0.9876526153536342445, 7.798540720466730171E-17 ) ) ;
#16613 = EDGE_LOOP ( 'NONE', ( #2367, #18474, #15580, #3143 ) ) ;
#16614 = AXIS2_PLACEMENT_3D ( 'NONE', #14143, #6967, #4183 ) ;
#16615 = DIRECTION ( 'NONE',  ( -0.1566598588826321192, 0.9876526153536342445, 7.798540720466730171E-17 ) ) ;
#16616 = FACE_BOUND ( 'NONE', #10908, .T. ) ;
#16617 = VECTOR ( 'NONE', #6244, 1000.000000000000000 ) ;
#16618 = DIRECTION ( 'NONE',  ( 0.000000000000000000, 0.000000000000000000, 1.000000000000000000 ) ) ;
#16619 = AXIS2_PLACEMENT_3D ( 'NONE', #11214, #2599, #12538 ) ;
#16620 = ORIENTED_EDGE ( 'NONE', *, *, #17484, .F. ) ;
#16621 = DIRECTION ( 'NONE',  ( -0.9201637183752250371, 0.3915338189555017112, -0.000000000000000000 ) ) ;
#16622 = CARTESIAN_POINT ( 'NONE',  ( -33.20773785067495254, -25.51714336811882688, -8.660254037844380193 ) ) ;
#16623 = CARTESIAN_POINT ( 'NONE',  ( -51.27495791377663181, -23.32042782179674845, 4.330127018922218518 ) ) ;
#16624 = ORIENTED_EDGE ( 'NONE', *, *, #17640, .F. ) ;
#16625 = ORIENTED_EDGE ( 'NONE', *, *, #15550, .F. ) ;
#16626 = FACE_OUTER_BOUND ( 'NONE', #16290, .T. ) ;
#16627 = CARTESIAN_POINT ( 'NONE',  ( 2.000000000000000000, 2.449293598294706414E-16, 30.00000000000000000 ) ) ;
#16628 = AXIS2_PLACEMENT_3D ( 'NONE', #210, #7512, #309 ) ;
#16629 = ORIENTED_EDGE ( 'NONE', *, *, #2761, .F. ) ;
#16630 = LINE ( 'NONE', #15201, #4871 ) ;
#16631 = AXIS2_PLACEMENT_3D ( 'NONE', #12795, #18722, #10041 ) ;
#16632 = EDGE_LOOP ( 'NONE', ( #17887, #14283 ) ) ;
#16633 = CARTESIAN_POINT ( 'NONE',  ( -30.73860631229088369, -25.12549372091224598, -12.99038105676658006 ) ) ;
#16634 = EDGE_CURVE ( 'NONE', #1595, #11742, #6331, .T. ) ;
#16635 = CARTESIAN_POINT ( 'NONE',  ( -169.4916495677151715, 31.92505963027457483, 3.278196957010509394 ) ) ;
#16636 = CIRCLE ( 'NONE', #11749, 1.500000000000000888 ) ;
#16637 = VERTEX_POINT ( 'NONE', #427 ) ;
#16638 = EDGE_CURVE ( 'NONE', #15242, #5250, #1659, .T. ) ;
#16639 = VECTOR ( 'NONE', #4597, 1000.000000000000000 ) ;
#16640 = CIRCLE ( 'NONE', #13879, 1.499999999999999556 ) ;
#16641 = CIRCLE ( 'NONE', #6054, 1.500000000000000888 ) ;
#16642 = DIRECTION ( 'NONE',  ( -0.9876526153536336894, -0.1566598588826349503, 0.000000000000000000 ) ) ;
#16643 = ADVANCED_FACE ( 'NONE', ( #16446 ), #11936, .F. ) ;
#16644 = CARTESIAN_POINT ( 'NONE',  ( 0.5768043922889515285, -15.09578523045857601, -8.660254037844383745 ) ) ;
#16645 = CARTESIAN_POINT ( 'NONE',  ( -28.22983976372896109, -82.43302551005379541, 21.65063509461101532 ) ) ;
#16646 = APPLICATION_PROTOCOL_DEFINITION ( 'draft international standard', 'automotive_design', 1998, #16966 ) ;
#16647 = ORIENTED_EDGE ( 'NONE', *, *, #10640, .F. ) ;
#16648 = VECTOR ( 'NONE', #14321, 1000.000000000000000 ) ;
#16649 = CIRCLE ( 'NONE', #7562, 2.500000000000002220 ) ;
#16650 = DIRECTION ( 'NONE',  ( -0.1566598588826321747, 0.9876526153536343555, 0.000000000000000000 ) ) ;
#16651 = DIRECTION ( 'NONE',  ( -0.1566598588826321747, 0.9876526153536343555, 0.000000000000000000 ) ) ;
#16652 = DIRECTION ( 'NONE',  ( -1.000000000000000000, 0.000000000000000000, 0.000000000000000000 ) ) ;
#16653 = DIRECTION ( 'NONE',  ( 1.000000000000000000, 0.000000000000000000, -2.671473304378624222E-16 ) ) ;
#16654 = VECTOR ( 'NONE', #11015, 1000.000000000000000 ) ;
#16655 = VERTEX_POINT ( 'NONE', #16345 ) ;
#16656 = ORIENTED_EDGE ( 'NONE', *, *, #978, .T. ) ;
#16657 = DIRECTION ( 'NONE',  ( -0.9876526153536336894, -0.1566598588826349503, 0.000000000000000000 ) ) ;
#16658 = ORIENTED_EDGE ( 'NONE', *, *, #12216, .F. ) ;
#16659 = AXIS2_PLACEMENT_3D ( 'NONE', #1019, #6982, #1201 ) ;
#16660 = DIRECTION ( 'NONE',  ( -0.1566598588826321192, 0.9876526153536342445, 7.798540720466730171E-17 ) ) ;
#16661 = ORIENTED_EDGE ( 'NONE', *, *, #2882, .T. ) ;
#16662 = VERTEX_POINT ( 'NONE', #512 ) ;
#16663 = ORIENTED_EDGE ( 'NONE', *, *, #9152, .T. ) ;
#16664 = VECTOR ( 'NONE', #14066, 1000.000000000000000 ) ;
#16665 = AXIS2_PLACEMENT_3D ( 'NONE', #1637, #16036, #7675 ) ;
#16666 = DIRECTION ( 'NONE',  ( -0.1566598588826321747, 0.9876526153536343555, 0.000000000000000000 ) ) ;
#16667 = ORIENTED_EDGE ( 'NONE', *, *, #3482, .T. ) ;
#16668 = CARTESIAN_POINT ( 'NONE',  ( -39.09401853261888959, -84.15628395776273862, 1.424741226644455312E-14 ) ) ;
#16669 = EDGE_CURVE ( 'NONE', #15242, #11338, #7438, .T. ) ;
#16670 = CARTESIAN_POINT ( 'NONE',  ( -0.1213752363283457369, -20.26903809555066616, 8.660254037844412167 ) ) ;
#16671 = AXIS2_PLACEMENT_3D ( 'NONE', #16960, #13992, #1044 ) ;
#16672 = VERTEX_POINT ( 'NONE', #9142 ) ;
#16673 = CARTESIAN_POINT ( 'NONE',  ( -33.00338452973448966, -20.42222043246805541, -12.99038105676658006 ) ) ;
#16674 = PRODUCT_DEFINITION_SHAPE ( 'NONE', 'NONE',  #8012 ) ;
#16675 = DIRECTION ( 'NONE',  ( -0.1566598588826321192, 0.9876526153536342445, 7.798540720466731404E-17 ) ) ;
#16676 = CARTESIAN_POINT ( 'NONE',  ( -46.50141314777111745, -85.33123289938247069, -21.65063509461098690 ) ) ;
#16677 = EDGE_CURVE ( 'NONE', #5722, #17580, #569, .T. ) ;
#16678 = CIRCLE ( 'NONE', #8501, 1.499999999999999556 ) ;
#16679 = CARTESIAN_POINT ( 'NONE',  ( -309.1404785418517918, -2.850701963179328668, 15.88900348692940945 ) ) ;
#16680 = DIRECTION ( 'NONE',  ( 1.000000000000000000, 0.000000000000000000, 0.000000000000000000 ) ) ;
#16681 = CIRCLE ( 'NONE', #12417, 1.499999999999997335 ) ;
#16682 = DIRECTION ( 'NONE',  ( -0.1566598588826321192, 0.9876526153536342445, 7.798540720466731404E-17 ) ) ;
#16683 = ORIENTED_EDGE ( 'NONE', *, *, #16977, .F. ) ;
#16684 = CIRCLE ( 'NONE', #16990, 1.499999999999999556 ) ;
#16685 = PLANE ( 'NONE',  #15951 ) ;
#16686 = ORIENTED_EDGE ( 'NONE', *, *, #2341, .T. ) ;
#16687 = CIRCLE ( 'NONE', #1855, 2.999999999999999112 ) ;
#16688 = FACE_OUTER_BOUND ( 'NONE', #12720, .T. ) ;
#16689 = EDGE_LOOP ( 'NONE', ( #4366, #2024 ) ) ;
#16690 = CIRCLE ( 'NONE', #947, 1.499999999999999556 ) ;
#16691 = CARTESIAN_POINT ( 'NONE',  ( -70.00000000000001421, 44.99999999999998579, 2.500000000000000000 ) ) ;
#16692 = CARTESIAN_POINT ( 'NONE',  ( -4.526176995241833367, -78.67318889687062722, -17.32050807568878525 ) ) ;
#16693 = CIRCLE ( 'NONE', #10895, 1.500000000000001332 ) ;
#16694 = CARTESIAN_POINT ( 'NONE',  ( -129.1404785418517918, 8.649298036820674440, -5.500000000000000000 ) ) ;
#16695 = VERTEX_POINT ( 'NONE', #11759 ) ;
#16696 = CYLINDRICAL_SURFACE ( 'NONE', #6394, 1.500000000000000666 ) ;
#16697 = CARTESIAN_POINT ( 'NONE',  ( -68.55887868246516348, -26.06197535224279349, -17.32050807568878170 ) ) ;
#16698 = DIRECTION ( 'NONE',  ( 0.000000000000000000, 0.000000000000000000, 1.000000000000000000 ) ) ;
#16699 = EDGE_CURVE ( 'NONE', #7569, #8040, #14643, .T. ) ;
#16700 = EDGE_CURVE ( 'NONE', #5412, #4610, #15998, .T. ) ;
#16701 = CARTESIAN_POINT ( 'NONE',  ( -86.18478963674542115, 32.34879426031891114, -35.00000000000000000 ) ) ;
#16702 = DIRECTION ( 'NONE',  ( -0.1566598588826321192, 0.9876526153536342445, 7.798540720466731404E-17 ) ) ;
#16703 = DIRECTION ( 'NONE',  ( -0.000000000000000000, -0.000000000000000000, -1.000000000000000000 ) ) ;
#16704 = ORIENTED_EDGE ( 'NONE', *, *, #8786, .F. ) ;
#16705 = ADVANCED_FACE ( 'NONE', ( #10649 ), #13197, .F. ) ;
#16706 = CARTESIAN_POINT ( 'NONE',  ( -172.7326993491721225, 43.83249341393818810, 9.951701414186830458E-16 ) ) ;
#16707 = CARTESIAN_POINT ( 'NONE',  ( -79.93235417334217630, 2.099789364928617452, 2.874262317885239781 ) ) ;
#16708 = AXIS2_PLACEMENT_3D ( 'NONE', #3004, #13499, #1606 ) ;
#16709 = DIRECTION ( 'NONE',  ( 2.887450008416415878E-16, 0.000000000000000000, 1.000000000000000000 ) ) ;
#16710 = VERTEX_POINT ( 'NONE', #13471 ) ;
#16711 = VERTEX_POINT ( 'NONE', #12040 ) ;
#16712 = ORIENTED_EDGE ( 'NONE', *, *, #15232, .T. ) ;
#16713 = FACE_OUTER_BOUND ( 'NONE', #17402, .T. ) ;
#16714 = AXIS2_PLACEMENT_3D ( 'NONE', #2259, #15161, #6268 ) ;
#16715 = FACE_BOUND ( 'NONE', #7427, .T. ) ;
#16716 = AXIS2_PLACEMENT_3D ( 'NONE', #4364, #3029, #8821 ) ;
#16717 = SURFACE_STYLE_FILL_AREA ( #12597 ) ;
#16718 = ORIENTED_EDGE ( 'NONE', *, *, #127, .T. ) ;
#16719 = AXIS2_PLACEMENT_3D ( 'NONE', #18378, #15661, #15954 ) ;
#16720 = ADVANCED_FACE ( 'NONE', ( #8944 ), #3262, .T. ) ;
#16721 = VERTEX_POINT ( 'NONE', #15005 ) ;
#16722 = CYLINDRICAL_SURFACE ( 'NONE', #9128, 1.500000000000001554 ) ;
#16723 = ORIENTED_EDGE ( 'NONE', *, *, #17292, .T. ) ;
#16724 = EDGE_CURVE ( 'NONE', #1063, #16044, #16243, .T. ) ;
#16725 = CIRCLE ( 'NONE', #2795, 1.500000000000000888 ) ;
#16726 = DIRECTION ( 'NONE',  ( -0.1566598588826321192, 0.9876526153536342445, 7.798540720466730171E-17 ) ) ;
#16727 = CARTESIAN_POINT ( 'NONE',  ( -7.528769851480577202, -21.44398703717040888, 4.330127018922214077 ) ) ;
#16728 = EDGE_CURVE ( 'NONE', #11102, #442, #14721, .T. ) ;
#16729 = CARTESIAN_POINT ( 'NONE',  ( 0.5768043922889515285, -15.09578523045857601, 17.32050807568881368 ) ) ;
#16730 = VECTOR ( 'NONE', #15334, 1000.000000000000000 ) ;
#16731 = EDGE_CURVE ( 'NONE', #7806, #1829, #328, .T. ) ;
#16732 = CARTESIAN_POINT ( 'NONE',  ( -29.05277406831996245, -19.79558099693753803, 8.660254037844417496 ) ) ;
#16733 = ORIENTED_EDGE ( 'NONE', *, *, #13827, .T. ) ;
#16734 = VERTEX_POINT ( 'NONE', #6682 ) ;
#16735 = LINE ( 'NONE', #9711, #18766 ) ;
#16736 = CARTESIAN_POINT ( 'NONE',  ( -168.8266622669028152, 31.94878367126290897, -2.822349119005427287 ) ) ;
#16737 = AXIS2_PLACEMENT_3D ( 'NONE', #17760, #9204, #8050 ) ;
#16738 = EDGE_LOOP ( 'NONE', ( #2069, #300 ) ) ;
#16739 = VERTEX_POINT ( 'NONE', #18275 ) ;
#16740 = DIRECTION ( 'NONE',  ( -0.1566598588826321747, 0.9876526153536343555, 0.000000000000000000 ) ) ;
#16741 = CARTESIAN_POINT ( 'NONE',  ( -2.590506774712417748, -20.66068774275724707, -12.99038105676658361 ) ) ;
#16742 = VERTEX_POINT ( 'NONE', #17014 ) ;
#16743 = CARTESIAN_POINT ( 'NONE',  ( 2.000000000000000000, 2.449293598294706414E-16, 30.00000000000000000 ) ) ;
#16744 = CARTESIAN_POINT ( 'NONE',  ( -167.4745151998187680, 32.15905408292213252, 2.500000000000000000 ) ) ;
#16745 = CYLINDRICAL_SURFACE ( 'NONE', #4850, 1.500000000000001554 ) ;
#16746 = CARTESIAN_POINT ( 'NONE',  ( -44.85521591397802155, -22.30213873905965372, 21.65063509461101887 ) ) ;
#16747 = DIRECTION ( 'NONE',  ( -0.1566598588826321747, 0.9876526153536343555, 0.000000000000000000 ) ) ;
#16748 =( NAMED_UNIT ( * ) PLANE_ANGLE_UNIT ( ) SI_UNIT ( $, .RADIAN. ) );
#16749 = DIRECTION ( 'NONE',  ( -3.039628882124824168E-17, -0.000000000000000000, 1.000000000000000000 ) ) ;
#16750 = CYLINDRICAL_SURFACE ( 'NONE', #6280, 1.500000000000001554 ) ;
#16751 = ADVANCED_FACE ( 'NONE', ( #15373 ), #14042, .F. ) ;
#16752 = CYLINDRICAL_SURFACE ( 'NONE', #6951, 1.500000000000001554 ) ;
#16753 = DIRECTION ( 'NONE',  ( -0.9876526153536336894, -0.1566598588826350336, 0.000000000000000000 ) ) ;
#16754 = CYLINDRICAL_SURFACE ( 'NONE', #12909, 1.500000000000001554 ) ;
#16755 = ORIENTED_EDGE ( 'NONE', *, *, #1797, .F. ) ;
#16756 = ADVANCED_FACE ( 'NONE', ( #5246 ), #2293, .F. ) ;
#16757 = ORIENTED_EDGE ( 'NONE', *, *, #16353, .F. ) ;
#16758 = CIRCLE ( 'NONE', #100, 1.500000000000001332 ) ;
#16759 = CARTESIAN_POINT ( 'NONE',  ( -62.00000000000000000, 0.000000000000000000, 25.00000000000000000 ) ) ;
#16760 = DIRECTION ( 'NONE',  ( -0.1566598588826321192, 0.9876526153536342445, 7.798540720466730171E-17 ) ) ;
#16761 = ORIENTED_EDGE ( 'NONE', *, *, #17993, .T. ) ;
#16762 = EDGE_LOOP ( 'NONE', ( #13846, #3343, #7074, #3634 ) ) ;
#16763 = ORIENTED_EDGE ( 'NONE', *, *, #467, .T. ) ;
#16764 = ORIENTED_EDGE ( 'NONE', *, *, #134, .F. ) ;
#16765 = EDGE_CURVE ( 'NONE', #3705, #10837, #7516, .T. ) ;
#16766 = CARTESIAN_POINT ( 'NONE',  ( -67.57122606711153878, -25.90531549336017036, 4.330127018922218518 ) ) ;
#16767 = ORIENTED_EDGE ( 'NONE', *, *, #7031, .F. ) ;
#16768 = ORIENTED_EDGE ( 'NONE', *, *, #10643, .F. ) ;
#16769 = DIRECTION ( 'NONE',  ( -0.1566598588826321192, 0.9876526153536342445, 7.798540720466730171E-17 ) ) ;
#16770 = DIRECTION ( 'NONE',  ( -0.9876526153536336894, -0.1566598588826349503, 0.000000000000000000 ) ) ;
#16771 = DIRECTION ( 'NONE',  ( -0.1566598588826321192, 0.9876526153536342445, 7.798540720466730171E-17 ) ) ;
#16772 = CYLINDRICAL_SURFACE ( 'NONE', #14215, 1.500000000000001554 ) ;
#16773 = ORIENTED_EDGE ( 'NONE', *, *, #2973, .T. ) ;
#16774 = DIRECTION ( 'NONE',  ( -0.9876526153536344665, -0.1566598588826304539, 0.000000000000000000 ) ) ;
#16775 = AXIS2_PLACEMENT_3D ( 'NONE', #18711, #5788, #15901 ) ;
#16776 = DIRECTION ( 'NONE',  ( -0.000000000000000000, -1.000000000000000000, -0.000000000000000000 ) ) ;
#16777 = ORIENTED_EDGE ( 'NONE', *, *, #6776, .T. ) ;
#16778 = CARTESIAN_POINT ( 'NONE',  ( 3.231158466157545206, -19.73726462726228092, 30.00000000000000000 ) ) ;
#16779 = EDGE_LOOP ( 'NONE', ( #7703, #16233 ) ) ;
#16780 = PLANE ( 'NONE',  #12047 ) ;
#16781 = FACE_OUTER_BOUND ( 'NONE', #10121, .T. ) ;
#16782 = EDGE_LOOP ( 'NONE', ( #5285, #17579, #18623, #16854 ) ) ;
#16783 = FACE_OUTER_BOUND ( 'NONE', #6148, .T. ) ;
#16784 = FACE_OUTER_BOUND ( 'NONE', #7709, .T. ) ;
#16785 = EDGE_LOOP ( 'NONE', ( #12307, #12847 ) ) ;
#16786 = DIRECTION ( 'NONE',  ( -0.1566598588826321747, 0.9876526153536343555, 0.000000000000000000 ) ) ;
#16787 = VECTOR ( 'NONE', #2155, 1000.000000000000000 ) ;
#16788 = ORIENTED_EDGE ( 'NONE', *, *, #9567, .T. ) ;
#16789 = EDGE_CURVE ( 'NONE', #5230, #16279, #8127, .T. ) ;
#16790 = VERTEX_POINT ( 'NONE', #1091 ) ;
#16791 = DIRECTION ( 'NONE',  ( -0.1566598588826321192, 0.9876526153536342445, 7.798540720466730171E-17 ) ) ;
#16792 = EDGE_CURVE ( 'NONE', #8719, #8399, #16735, .T. ) ;
#16793 = ORIENTED_EDGE ( 'NONE', *, *, #11038, .T. ) ;
#16794 = DIRECTION ( 'NONE',  ( 0.000000000000000000, 0.000000000000000000, 1.000000000000000000 ) ) ;
#16795 = DIRECTION ( 'NONE',  ( 0.000000000000000000, 0.000000000000000000, 1.000000000000000000 ) ) ;
#16796 = EDGE_CURVE ( 'NONE', #17807, #7902, #9929, .T. ) ;
#16797 = CARTESIAN_POINT ( 'NONE',  ( -51.43967622453926936, -86.11453219379562540, -21.65063509461098690 ) ) ;
#16798 = ORIENTED_EDGE ( 'NONE', *, *, #357, .T. ) ;
#16799 = CYLINDRICAL_SURFACE ( 'NONE', #15178, 2.200000000000000178 ) ;
#16800 = DIRECTION ( 'NONE',  ( -0.1566598588826321192, 0.9876526153536342445, 7.798540720466730171E-17 ) ) ;
#16801 = PLANE ( 'NONE',  #18151 ) ;
#16802 = LINE ( 'NONE', #10880, #8361 ) ;
#16803 = EDGE_LOOP ( 'NONE', ( #4765, #9753, #7265, #4625, #5877, #10959, #6926 ) ) ;
#16804 = DIRECTION ( 'NONE',  ( -0.1566598588826321192, 0.9876526153536342445, 7.798540720466730171E-17 ) ) ;
#16805 = CARTESIAN_POINT ( 'NONE',  ( -32.50955822205765600, -20.34389050302674917, 1.926565525561697761E-14 ) ) ;
#16806 = EDGE_CURVE ( 'NONE', #2279, #16410, #16823, .T. ) ;
#16807 = CARTESIAN_POINT ( 'NONE',  ( -6.326550248787502032E-15, -2.199999999999977085, -130.3485206753969976 ) ) ;
#16808 = ORIENTED_EDGE ( 'NONE', *, *, #11997, .T. ) ;
#16809 = ORIENTED_EDGE ( 'NONE', *, *, #17837, .T. ) ;
#16810 = DIRECTION ( 'NONE',  ( 0.000000000000000000, 0.000000000000000000, 1.000000000000000000 ) ) ;
#16811 = EDGE_CURVE ( 'NONE', #11250, #113, #7254, .T. ) ;
#16812 = FACE_BOUND ( 'NONE', #17287, .T. ) ;
#16813 = ADVANCED_FACE ( 'NONE', ( #2499 ), #12608, .F. ) ;
#16814 = VECTOR ( 'NONE', #9006, 1000.000000000000000 ) ;
#16815 = EDGE_LOOP ( 'NONE', ( #3224, #16029, #1187, #15218 ) ) ;
#16816 = CARTESIAN_POINT ( 'NONE',  ( -36.46016868347218320, -20.97052993855726655, -12.99038105676658006 ) ) ;
#16817 = CARTESIAN_POINT ( 'NONE',  ( -22.63303206852135929, -18.77729191420043620, 17.32050807568881723 ) ) ;
#16818 = VERTEX_POINT ( 'NONE', #18465 ) ;
#16819 = DIRECTION ( 'NONE',  ( 0.000000000000000000, 0.000000000000000000, 1.000000000000000000 ) ) ;
#16820 = DIRECTION ( 'NONE',  ( 0.000000000000000000, 0.000000000000000000, 1.000000000000000000 ) ) ;
#16821 = CARTESIAN_POINT ( 'NONE',  ( 2.200000000000000178, 2.694222958124177006E-16, 25.00000000000000000 ) ) ;
#16822 = EDGE_LOOP ( 'NONE', ( #16022, #3351, #16009, #18545 ) ) ;
#16823 = LINE ( 'NONE', #796, #10534 ) ;
#16824 = CIRCLE ( 'NONE', #4679, 1.500000000000001332 ) ;
#16825 = DIRECTION ( 'NONE',  ( -0.1566598588826321192, 0.9876526153536342445, 7.798540720466730171E-17 ) ) ;
#16826 = EDGE_CURVE ( 'NONE', #11894, #1825, #13665, .T. ) ;
#16827 = CARTESIAN_POINT ( 'NONE',  ( -11.93357161039406300, -79.84813783849037350, 21.65063509461100821 ) ) ;
#16828 = EDGE_LOOP ( 'NONE', ( #456, #17962 ) ) ;
#16829 = ORIENTED_EDGE ( 'NONE', *, *, #4013, .T. ) ;
#16830 = CARTESIAN_POINT ( 'NONE',  ( -13.45468554360235203, -22.38394619046619383, -8.660254037844380193 ) ) ;
#16831 = ADVANCED_BREP_SHAPE_REPRESENTATION ( '', ( #14964, #18772 ), #5087 ) ;
#16832 = EDGE_CURVE ( 'NONE', #15217, #14719, #9664, .T. ) ;
#16833 = EDGE_CURVE ( 'NONE', #8732, #10693, #9336, .T. ) ;
#16834 = DIRECTION ( 'NONE',  ( -0.000000000000000000, -0.000000000000000000, -1.000000000000000000 ) ) ;
#16835 = DIRECTION ( 'NONE',  ( -0.1566598588826321747, 0.9876526153536343555, 0.000000000000000000 ) ) ;
#16836 = ORIENTED_EDGE ( 'NONE', *, *, #11658, .F. ) ;
#16837 = PRODUCT_DEFINITION_SHAPE ( 'NONE', 'NONE',  #2110 ) ;
#16838 = FACE_BOUND ( 'NONE', #3383, .T. ) ;
#16839 = FACE_OUTER_BOUND ( 'NONE', #2502, .T. ) ;
#16840 = VECTOR ( 'NONE', #3910, 1000.000000000000000 ) ;
#16841 = CARTESIAN_POINT ( 'NONE',  ( -74.31763473078903814, 46.83717308261807943, 2.499999999999997780 ) ) ;
#16842 = DIRECTION ( 'NONE',  ( 1.000000000000000000, 0.000000000000000000, 0.000000000000000000 ) ) ;
#16843 = DIRECTION ( 'NONE',  ( -0.9876526153536336894, -0.1566598588826349503, 0.000000000000000000 ) ) ;
#16844 = CARTESIAN_POINT ( 'NONE',  ( -33.99103714508810725, -20.57888029135068564, -17.32050807568878170 ) ) ;
#16845 = CARTESIAN_POINT ( 'NONE',  ( -7.818242838216901802, -16.42739403096095074, 8.660254037844413944 ) ) ;
#16846 = DIRECTION ( 'NONE',  ( -0.9826218788918642533, -0.1856185419698762884, 0.000000000000000000 ) ) ;
#16847 = ORIENTED_EDGE ( 'NONE', *, *, #7662, .F. ) ;
#16848 = ORIENTED_EDGE ( 'NONE', *, *, #812, .T. ) ;
#16849 = DIRECTION ( 'NONE',  ( 0.000000000000000000, 0.000000000000000000, 1.000000000000000000 ) ) ;
#16850 = CARTESIAN_POINT ( 'NONE',  ( -41.39843176024034221, -21.75382923297042481, -12.99038105676658006 ) ) ;
#16851 = TOROIDAL_SURFACE ( 'NONE', #17454, 12.83663829214476060, 3.000000000000000000 ) ;
#16852 = ORIENTED_EDGE ( 'NONE', *, *, #7189, .F. ) ;
#16853 = AXIS2_PLACEMENT_3D ( 'NONE', #4257, #10311, #2749 ) ;
#16854 = ORIENTED_EDGE ( 'NONE', *, *, #6802, .T. ) ;
#16855 = CARTESIAN_POINT ( 'NONE',  ( -56.37793930130741415, -86.89783148820880854, 12.99038105676661203 ) ) ;
#16856 = CARTESIAN_POINT ( 'NONE',  ( 0.3724510713484854851, -20.19070816610934926, 21.65063509461101177 ) ) ;
#16857 = DIRECTION ( 'NONE',  ( 0.000000000000000000, 0.000000000000000000, 1.000000000000000000 ) ) ;
#16858 = ADVANCED_FACE ( 'NONE', ( #16626 ), #16921, .F. ) ;
#16859 = ORIENTED_EDGE ( 'NONE', *, *, #16069, .F. ) ;
#16860 = CARTESIAN_POINT ( 'NONE',  ( -46.33669483700847280, -22.53712852738359018, 4.330127018922218518 ) ) ;
#16861 = EDGE_CURVE ( 'NONE', #5480, #16555, #1496, .T. ) ;
#16862 = VECTOR ( 'NONE', #5708, 1000.000000000000000 ) ;
#16863 = DIRECTION ( 'NONE',  ( -0.000000000000000000, -0.000000000000000000, -1.000000000000000000 ) ) ;
#16864 = FACE_OUTER_BOUND ( 'NONE', #12150, .T. ) ;
#16865 = SURFACE_STYLE_USAGE ( .BOTH. , #18315 ) ;
#16866 = DIRECTION ( 'NONE',  ( -0.9876526153536341335, -0.1566598588826327021, 0.000000000000000000 ) ) ;
#16867 = AXIS2_PLACEMENT_3D ( 'NONE', #13341, #16569, #4621 ) ;
#16868 = ORIENTED_EDGE ( 'NONE', *, *, #2660, .F. ) ;
#16869 = CARTESIAN_POINT ( 'NONE',  ( -26.78799585087635649, -24.49885428538171794, -17.32050807568878170 ) ) ;
#16870 = DIRECTION ( 'NONE',  ( -0.1566598588826321192, 0.9876526153536342445, 7.798540720466730171E-17 ) ) ;
#16871 = ORIENTED_EDGE ( 'NONE', *, *, #14755, .T. ) ;
#16872 = CARTESIAN_POINT ( 'NONE',  ( -21.64537945316773460, -18.62063205531779886, 12.99038105676661736 ) ) ;
#16873 = ORIENTED_EDGE ( 'NONE', *, *, #16826, .T. ) ;
#16874 = VERTEX_POINT ( 'NONE', #3608 ) ;
#16875 = CARTESIAN_POINT ( 'NONE',  ( -1.892327146095121204, -15.48743487766515337, 4.330127018922213189 ) ) ;
#16876 = ORIENTED_EDGE ( 'NONE', *, *, #15330, .F. ) ;
#16877 = AXIS2_PLACEMENT_3D ( 'NONE', #9862, #7324, #104 ) ;
#16878 = CARTESIAN_POINT ( 'NONE',  ( 3.231158466157551423, 19.73726462726227737, 30.00000000000000000 ) ) ;
#16879 = FACE_OUTER_BOUND ( 'NONE', #2120, .T. ) ;
#16880 = DIRECTION ( 'NONE',  ( 0.000000000000000000, 0.000000000000000000, 1.000000000000000000 ) ) ;
#16881 = VERTEX_POINT ( 'NONE', #2207 ) ;
#16882 = VECTOR ( 'NONE', #8686, 1000.000000000000114 ) ;
#16883 = CARTESIAN_POINT ( 'NONE',  ( 0.000000000000000000, 0.000000000000000000, -30.00000000000000000 ) ) ;
#16884 = AXIS2_PLACEMENT_3D ( 'NONE', #15967, #11496, #11669 ) ;
#16885 = LINE ( 'NONE', #6542, #12175 ) ;
#16886 = CIRCLE ( 'NONE', #5369, 1.500000000000001332 ) ;
#16887 = CARTESIAN_POINT ( 'NONE',  ( 0.5768043922889515285, -15.09578523045857601, 8.660254037844412167 ) ) ;
#16888 = CARTESIAN_POINT ( 'NONE',  ( -170.4124675745486570, 31.54971992778987655, -2.500000000000000000 ) ) ;
#16889 = VECTOR ( 'NONE', #9651, 1000.000000000000000 ) ;
#16890 = EDGE_CURVE ( 'NONE', #11171, #10712, #4504, .T. ) ;
#16891 = DIRECTION ( 'NONE',  ( -0.9876526153536341335, -0.1566598588826327021, 0.000000000000000000 ) ) ;
#16892 = CARTESIAN_POINT ( 'NONE',  ( -66.08974714408108753, -25.67032570503622679, 12.99038105676661736 ) ) ;
#16893 = DIRECTION ( 'NONE',  ( 0.000000000000000000, 0.000000000000000000, 1.000000000000000000 ) ) ;
#16894 = DIRECTION ( 'NONE',  ( -0.1566598588826321192, 0.9876526153536342445, 7.798540720466731404E-17 ) ) ;
#16895 = VECTOR ( 'NONE', #9988, 1000.000000000000000 ) ;
#16896 = COLOUR_RGB ( '', 0.66274510, 0.83137255, 0.94901961) ;
#16897 = FACE_OUTER_BOUND ( 'NONE', #17024, .T. ) ;
#16898 = EDGE_CURVE ( 'NONE', #8532, #8941, #3271, .T. ) ;
#16899 = ORIENTED_EDGE ( 'NONE', *, *, #12042, .F. ) ;
#16900 = DIRECTION ( 'NONE',  ( 0.000000000000000000, 0.000000000000000000, 1.000000000000000000 ) ) ;
#16901 = EDGE_LOOP ( 'NONE', ( #11698, #16712 ) ) ;
#16902 = ORIENTED_EDGE ( 'NONE', *, *, #14636, .F. ) ;
#16903 = CARTESIAN_POINT ( 'NONE',  ( 2.841582609732560272, -19.79905851890276836, 8.660254037844412167 ) ) ;
#16904 = VECTOR ( 'NONE', #6841, 1000.000000000000000 ) ;
#16905 = FACE_BOUND ( 'NONE', #689, .T. ) ;
#16906 = VERTEX_POINT ( 'NONE', #1184 ) ;
#16907 = AXIS2_PLACEMENT_3D ( 'NONE', #15446, #18437, #6547 ) ;
#16908 = ADVANCED_FACE ( 'NONE', ( #7341 ), #1552, .F. ) ;
#16909 = DIRECTION ( 'NONE',  ( -0.1566598588826321747, 0.9876526153536343555, 0.000000000000000000 ) ) ;
#16910 = FACE_BOUND ( 'NONE', #692, .T. ) ;
#16911 = ORIENTED_EDGE ( 'NONE', *, *, #15415, .T. ) ;
#16912 = CARTESIAN_POINT ( 'NONE',  ( -16.70711637639958269, -17.83733276090463704, 12.99038105676661381 ) ) ;
#16913 = VECTOR ( 'NONE', #15909, 1000.000000000000000 ) ;
#16914 = DIRECTION ( 'NONE',  ( -0.1566598588826321192, 0.9876526153536342445, 7.798540720466731404E-17 ) ) ;
#16915 = CARTESIAN_POINT ( 'NONE',  ( 6.338001773648100468, -76.94993044916168401, -4.330127018922189208 ) ) ;
#16916 = EDGE_CURVE ( 'NONE', #5805, #11320, #18492, .T. ) ;
#16917 = CYLINDRICAL_SURFACE ( 'NONE', #3171, 1.500000000000001554 ) ;
#16918 = AXIS2_PLACEMENT_3D ( 'NONE', #13815, #10878, #4994 ) ;
#16919 = VERTEX_POINT ( 'NONE', #17303 ) ;
#16920 = CIRCLE ( 'NONE', #606, 1.500000000000001332 ) ;
#16921 = CYLINDRICAL_SURFACE ( 'NONE', #14790, 1.500000000000001554 ) ;
#16922 = AXIS2_PLACEMENT_3D ( 'NONE', #6242, #652, #3458 ) ;
#16923 = CARTESIAN_POINT ( 'NONE',  ( -170.5500457218257679, 32.36841325234162525, -5.132545408516862473 ) ) ;
#16924 = ORIENTED_EDGE ( 'NONE', *, *, #3926, .F. ) ;
#16925 = EDGE_LOOP ( 'NONE', ( #14486, #14098, #17019, #13221 ) ) ;
#16926 = DIRECTION ( 'NONE',  ( -1.000000000000000000, 0.000000000000000000, 0.000000000000000000 ) ) ;
#16927 = ORIENTED_EDGE ( 'NONE', *, *, #8063, .T. ) ;
#16928 = ORIENTED_EDGE ( 'NONE', *, *, #4087, .F. ) ;
#16929 = CARTESIAN_POINT ( 'NONE',  ( -128.7747222983995528, -14.93194821374235559, 4.051035741711868532 ) ) ;
#16930 = CARTESIAN_POINT ( 'NONE',  ( -56.41757431148526081, -29.19865005186066753, 1.887572821959364500E-14 ) ) ;
#16931 = AXIS2_PLACEMENT_3D ( 'NONE', #1841, #7530, #4940 ) ;
#16932 = AXIS2_PLACEMENT_3D ( 'NONE', #11533, #13235, #1 ) ;
#16933 = CARTESIAN_POINT ( 'NONE',  ( -70.61510477223565374, 45.26172985928680959, 4.986359585138714579 ) ) ;
#16934 = DIRECTION ( 'NONE',  ( -1.132965874902867903E-16, -8.542786370627488692E-17, 1.000000000000000000 ) ) ;
#16935 = EDGE_CURVE ( 'NONE', #2537, #1132, #17391, .T. ) ;
#16936 = EDGE_CURVE ( 'NONE', #13430, #4362, #8738, .T. ) ;
#16937 = CARTESIAN_POINT ( 'NONE',  ( -3.538524379888211335, -78.51652903798800764, -12.99038105676658539 ) ) ;
#16938 = LINE ( 'NONE', #18482, #520 ) ;
#16939 = ADVANCED_FACE ( 'NONE', ( #1283 ), #11376, .F. ) ;
#16940 = DIRECTION ( 'NONE',  ( -0.9876526153536341335, -0.1566598588826327021, 0.000000000000000000 ) ) ;
#16941 = VERTEX_POINT ( 'NONE', #14340 ) ;
#16942 = ORIENTED_EDGE ( 'NONE', *, *, #10277, .F. ) ;
#16943 = FACE_BOUND ( 'NONE', #15708, .T. ) ;
#16944 = CYLINDRICAL_SURFACE ( 'NONE', #5808, 1.500000000000000888 ) ;
#16945 = ORIENTED_EDGE ( 'NONE', *, *, #4912, .T. ) ;
#16946 = EDGE_CURVE ( 'NONE', #14599, #1993, #4794, .T. ) ;
#16947 = AXIS2_PLACEMENT_3D ( 'NONE', #10146, #11468, #4286 ) ;
#16948 = VERTEX_POINT ( 'NONE', #12993 ) ;
#16949 = PRODUCT_DEFINITION ( 'UNKNOWN', '', #4168, #3390 ) ;
#16950 = ORIENTED_EDGE ( 'NONE', *, *, #8584, .F. ) ;
#16951 = VECTOR ( 'NONE', #12648, 1000.000000000000000 ) ;
#16952 = FACE_OUTER_BOUND ( 'NONE', #7559, .T. ) ;
#16953 = VECTOR ( 'NONE', #7577, 1000.000000000000000 ) ;
#16954 = EDGE_LOOP ( 'NONE', ( #9540, #7318, #10293, #12735, #12877 ) ) ;
#16955 = CARTESIAN_POINT ( 'NONE',  ( -5.513829610595458064, -78.82984875575326100, 12.99038105676660848 ) ) ;
#16956 = CARTESIAN_POINT ( 'NONE',  ( -3.578159390066044665, -20.81734760163988440, 1.522258424776792809E-14 ) ) ;
#16957 = ORIENTED_EDGE ( 'NONE', *, *, #5812, .F. ) ;
#16958 = VECTOR ( 'NONE', #14731, 1000.000000000000000 ) ;
#16959 = CARTESIAN_POINT ( 'NONE',  ( 0.000000000000000000, 0.000000000000000000, -20.00000000000000355 ) ) ;
#16960 = CARTESIAN_POINT ( 'NONE',  ( -6.047290928450125946, -21.20899724884646531, -12.99038105676658006 ) ) ;
#16961 = LINE ( 'NONE', #15223, #15854 ) ;
#16962 = DIRECTION ( 'NONE',  ( -0.1566598588826321192, 0.9876526153536342445, 7.798540720466730171E-17 ) ) ;
#16963 = PRESENTATION_STYLE_ASSIGNMENT (( #5074 ) ) ;
#16964 = CIRCLE ( 'NONE', #11765, 1.499999999999999556 ) ;
#16965 = EDGE_CURVE ( 'NONE', #4998, #5711, #15081, .T. ) ;
#16966 = APPLICATION_CONTEXT ( 'automotive_design' ) ;
#16967 = DIRECTION ( 'NONE',  ( -0.1566598588826321192, 0.9876526153536342445, 7.798540720466730171E-17 ) ) ;
#16968 = AXIS2_PLACEMENT_3D ( 'NONE', #15702, #11516, #17350 ) ;
#16969 = ORIENTED_EDGE ( 'NONE', *, *, #4862, .T. ) ;
#16970 = CARTESIAN_POINT ( 'NONE',  ( -126.1404785418517918, 9.595891400605989219, -2.500000000000000000 ) ) ;
#16971 = FACE_OUTER_BOUND ( 'NONE', #4608, .T. ) ;
#16972 = DIRECTION ( 'NONE',  ( -0.1566598588826321192, 0.9876526153536342445, 7.798540720466730171E-17 ) ) ;
#16973 = PRODUCT_RELATED_PRODUCT_CATEGORY ( 'part', '', ( #454 ) ) ;
#16974 = DIRECTION ( 'NONE',  ( -0.000000000000000000, -0.000000000000000000, -1.000000000000000000 ) ) ;
#16975 = ORIENTED_EDGE ( 'NONE', *, *, #12515, .F. ) ;
#16976 = ADVANCED_FACE ( 'NONE', ( #2944 ), #18654, .F. ) ;
#16977 = EDGE_CURVE ( 'NONE', #11803, #227, #10256, .T. ) ;
#16978 = AXIS2_PLACEMENT_3D ( 'NONE', #15448, #9672, #3957 ) ;
#16979 = ORIENTED_EDGE ( 'NONE', *, *, #787, .F. ) ;
#16980 = AXIS2_PLACEMENT_3D ( 'NONE', #7713, #17781, #16237 ) ;
#16981 = AXIS2_PLACEMENT_3D ( 'NONE', #5106, #16702, #14971 ) ;
#16982 = CARTESIAN_POINT ( 'NONE',  ( -25.80034323552273534, -24.34219442649909126, 21.65063509461101887 ) ) ;
#16983 = CARTESIAN_POINT ( 'NONE',  ( -170.5980861165185445, 32.53234180668174247, 5.500000000000001776 ) ) ;
#16984 = CARTESIAN_POINT ( 'NONE',  ( -1.892327146095121204, -15.48743487766515337, 21.65063509461101532 ) ) ;
#16985 = CARTESIAN_POINT ( 'NONE',  ( -129.1404785418517918, 52.54032238931508658, 2.500000000000000000 ) ) ;
#16986 = AXIS2_PLACEMENT_3D ( 'NONE', #9921, #15707, #2734 ) ;
#16987 = DIRECTION ( 'NONE',  ( -0.1566598588826321192, 0.9876526153536342445, 7.798540720466731404E-17 ) ) ;
#16988 = VECTOR ( 'NONE', #1549, 1000.000000000000000 ) ;
#16989 = DIRECTION ( 'NONE',  ( -0.1566598588826321192, 0.9876526153536342445, 7.798540720466731404E-17 ) ) ;
#16990 = AXIS2_PLACEMENT_3D ( 'NONE', #17102, #7144, #13090 ) ;
#16991 = DIRECTION ( 'NONE',  ( -0.9876526153536336894, -0.1566598588826349503, 0.000000000000000000 ) ) ;
#16992 = AXIS2_PLACEMENT_3D ( 'NONE', #675, #18036, #10769 ) ;
#16993 = EDGE_CURVE ( 'NONE', #2654, #13520, #3874, .T. ) ;
#16994 = DIRECTION ( 'NONE',  ( -0.1566598588826321747, 0.9876526153536343555, 0.000000000000000000 ) ) ;
#16995 = ADVANCED_FACE ( 'NONE', ( #12893 ), #9873, .F. ) ;
#16996 = ORIENTED_EDGE ( 'NONE', *, *, #1355, .T. ) ;
#16997 = VERTEX_POINT ( 'NONE', #5721 ) ;
#16998 = VECTOR ( 'NONE', #1664, 1000.000000000000000 ) ;
#16999 = VERTEX_POINT ( 'NONE', #5532 ) ;
#17000 = CARTESIAN_POINT ( 'NONE',  ( -26.58364252993588650, -19.40393134973096068, 12.99038105676661736 ) ) ;
#17001 = EDGE_CURVE ( 'NONE', #3359, #8246, #11286, .T. ) ;
#17002 = VECTOR ( 'NONE', #17430, 1000.000000000000000 ) ;
#17003 = FACE_BOUND ( 'NONE', #13096, .T. ) ;
#17004 = AXIS2_PLACEMENT_3D ( 'NONE', #9535, #8499, #14284 ) ;
#17005 = DIRECTION ( 'NONE',  ( -0.1566598588826321192, 0.9876526153536342445, 7.798540720466731404E-17 ) ) ;
#17006 = DIRECTION ( 'NONE',  ( -0.9876526153536341335, -0.1566598588826327021, 0.000000000000000000 ) ) ;
#17007 = ORIENTED_EDGE ( 'NONE', *, *, #14405, .F. ) ;
#17008 = ORIENTED_EDGE ( 'NONE', *, *, #6638, .F. ) ;
#17009 = VECTOR ( 'NONE', #2637, 1000.000000000000000 ) ;
#17010 = DIRECTION ( 'NONE',  ( -0.1566598588826321192, 0.9876526153536342445, 7.798540720466730171E-17 ) ) ;
#17011 = FACE_OUTER_BOUND ( 'NONE', #6036, .T. ) ;
#17012 = CARTESIAN_POINT ( 'NONE',  ( -63.82496892663746735, -30.37359899348040315, -12.99038105676658006 ) ) ;
#17013 = DIRECTION ( 'NONE',  ( -0.1566598588826321747, 0.9876526153536343555, 0.000000000000000000 ) ) ;
#17014 = CARTESIAN_POINT ( 'NONE',  ( -44.85521591397803576, -22.30213873905964306, -4.330127018922180326 ) ) ;
#17015 = VECTOR ( 'NONE', #1287, 1000.000000000000000 ) ;
#17016 = ORIENTED_EDGE ( 'NONE', *, *, #15705, .T. ) ;
#17017 = AXIS2_PLACEMENT_3D ( 'NONE', #2123, #716, #6497 ) ;
#17018 = ORIENTED_EDGE ( 'NONE', *, *, #14640, .F. ) ;
#17019 = ORIENTED_EDGE ( 'NONE', *, *, #1372, .T. ) ;
#17020 = CYLINDRICAL_SURFACE ( 'NONE', #1567, 1.500000000000001554 ) ;
#17021 = EDGE_CURVE ( 'NONE', #6176, #10934, #16314, .T. ) ;
#17022 = ORIENTED_EDGE ( 'NONE', *, *, #18157, .F. ) ;
#17023 = ORIENTED_EDGE ( 'NONE', *, *, #10838, .F. ) ;
#17024 = EDGE_LOOP ( 'NONE', ( #16235, #6495, #7593, #11899 ) ) ;
#17025 = DIRECTION ( 'NONE',  ( -0.9876526153536344665, -0.1566598588826304539, 0.000000000000000000 ) ) ;
#17026 = CIRCLE ( 'NONE', #6105, 1.500000000000000888 ) ;
#17027 = CIRCLE ( 'NONE', #1886, 1.500000000000001332 ) ;
#17028 = CARTESIAN_POINT ( 'NONE',  ( -22.63303206852135929, -18.77729191420042909, -8.660254037844380193 ) ) ;
#17029 = ORIENTED_EDGE ( 'NONE', *, *, #7503, .F. ) ;
#17030 = EDGE_CURVE ( 'NONE', #10706, #8349, #8446, .T. ) ;
#17031 = VECTOR ( 'NONE', #7214, 1000.000000000000000 ) ;
#17032 = UNCERTAINTY_MEASURE_WITH_UNIT (LENGTH_MEASURE( 1.000000000000000082E-05 ), #16173, 'distance_accuracy_value', 'NONE');
#17033 = FACE_OUTER_BOUND ( 'NONE', #10104, .T. ) ;
#17034 = CARTESIAN_POINT ( 'NONE',  ( -15.92381708198643153, -22.77559583767277473, -4.330127018922181215 ) ) ;
#17035 = SHAPE_DEFINITION_REPRESENTATION ( #11205, #13723 ) ;
#17036 = DIRECTION ( 'NONE',  ( -0.9876526153536336894, -0.1566598588826349503, 0.000000000000000000 ) ) ;
#17037 = DIRECTION ( 'NONE',  ( -0.1566598588826321747, 0.9876526153536343555, 0.000000000000000000 ) ) ;
#17038 = AXIS2_PLACEMENT_3D ( 'NONE', #3582, #3683, #874 ) ;
#17039 = CARTESIAN_POINT ( 'NONE',  ( 2.058283315319403783, -14.86079544213463066, 8.660254037844412167 ) ) ;
#17040 = ORIENTED_EDGE ( 'NONE', *, *, #5567, .F. ) ;
#17041 = EDGE_LOOP ( 'NONE', ( #14631, #2242 ) ) ;
#17042 = DIRECTION ( 'NONE',  ( 1.000000000000000000, 0.000000000000000000, 0.000000000000000000 ) ) ;
#17043 = CARTESIAN_POINT ( 'NONE',  ( -30.73860631229088369, -25.12549372091224598, -21.65063509461098334 ) ) ;
#17044 = CARTESIAN_POINT ( 'NONE',  ( -10.45209268736360997, -79.61314805016641571, 4.330127018922213189 ) ) ;
#17045 = ORIENTED_EDGE ( 'NONE', *, *, #18409, .F. ) ;
#17046 = AXIS2_PLACEMENT_3D ( 'NONE', #261, #5687, #15999 ) ;
#17047 = DIRECTION ( 'NONE',  ( 1.000000000000000000, -0.000000000000000000, -0.000000000000000000 ) ) ;
#17048 = EDGE_LOOP ( 'NONE', ( #14326, #7049, #15754, #10602 ) ) ;
#17049 = CARTESIAN_POINT ( 'NONE',  ( 0.000000000000000000, 0.000000000000000000, -40.65685424949239035 ) ) ;
#17050 = EDGE_CURVE ( 'NONE', #13155, #3602, #11731, .T. ) ;
#17051 = EDGE_CURVE ( 'NONE', #12234, #10192, #15848, .T. ) ;
#17052 = DIRECTION ( 'NONE',  ( -0.9876526153536336894, -0.1566598588826349503, 0.000000000000000000 ) ) ;
#17053 = EDGE_CURVE ( 'NONE', #8527, #7443, #6016, .T. ) ;
#17054 = CARTESIAN_POINT ( 'NONE',  ( -126.5488609203928831, 9.603162112694475283, 2.499999999999999112 ) ) ;
#17055 = CARTESIAN_POINT ( 'NONE',  ( -72.50948914387967648, -26.68861478777331797, -21.65063509461098334 ) ) ;
#17056 = DIRECTION ( 'NONE',  ( -1.000000000000000000, 0.000000000000000000, 0.000000000000000000 ) ) ;
#17057 = DIRECTION ( 'NONE',  ( 1.000000000000000000, 0.000000000000000000, 0.000000000000000000 ) ) ;
#17058 = DIRECTION ( 'NONE',  ( 0.000000000000000000, 1.000000000000000000, 0.000000000000000000 ) ) ;
#17059 = EDGE_LOOP ( 'NONE', ( #17623, #5494, #4653, #277 ) ) ;
#17060 = DIRECTION ( 'NONE',  ( -0.9201637183752248150, 0.3915338189555022108, 0.000000000000000000 ) ) ;
#17061 = DIRECTION ( 'NONE',  ( -0.1566598588826321192, 0.9876526153536342445, 7.798540720466730171E-17 ) ) ;
#17062 = CYLINDRICAL_SURFACE ( 'NONE', #13207, 2.000000000000000000 ) ;
#17063 = VERTEX_POINT ( 'NONE', #14619 ) ;
#17064 = CARTESIAN_POINT ( 'NONE',  ( -83.11589401185503334, 30.91643816065307959, 35.00001200000000523 ) ) ;
#17066 = ORIENTED_EDGE ( 'NONE', *, *, #3119, .F. ) ;
#17065 = CARTESIAN_POINT ( 'NONE',  ( -63.62061560569701157, -25.27867605782964233, 1.908195823574487804E-14 ) ) ;
#17067 = ADVANCED_FACE ( 'NONE', ( #1996 ), #2378, .T. ) ;
#17068 = ORIENTED_EDGE ( 'NONE', *, *, #16457, .T. ) ;
#17069 = ORIENTED_EDGE ( 'NONE', *, *, #5449, .F. ) ;
#17070 = ADVANCED_FACE ( 'NONE', ( #400 ), #4462, .F. ) ;
#17071 = EDGE_CURVE ( 'NONE', #370, #12897, #588, .T. ) ;
#17072 = CIRCLE ( 'NONE', #8875, 1.500000000000000888 ) ;
#17073 = ORIENTED_EDGE ( 'NONE', *, *, #7737, .T. ) ;
#17074 = LINE ( 'NONE', #14202, #8829 ) ;
#17075 = ORIENTED_EDGE ( 'NONE', *, *, #8638, .T. ) ;
#17076 = DIRECTION ( 'NONE',  ( -0.1566598588826321192, 0.9876526153536342445, 7.798540720466730171E-17 ) ) ;
#17077 = DIRECTION ( 'NONE',  ( 0.000000000000000000, 0.000000000000000000, -1.000000000000000000 ) ) ;
#17078 = CYLINDRICAL_SURFACE ( 'NONE', #15795, 1.500000000000001554 ) ;
#17079 = LINE ( 'NONE', #1066, #11112 ) ;
#17080 = FACE_OUTER_BOUND ( 'NONE', #4674, .T. ) ;
#17081 = CYLINDRICAL_SURFACE ( 'NONE', #1706, 150.0000000000000284 ) ;
#17082 = DIRECTION ( 'NONE',  ( -0.9876526153536336894, -0.1566598588826349503, 0.000000000000000000 ) ) ;
#17083 = CIRCLE ( 'NONE', #1043, 2.000000000000000000 ) ;
#17084 = ORIENTED_EDGE ( 'NONE', *, *, #15772, .F. ) ;
#17085 = ORIENTED_EDGE ( 'NONE', *, *, #10702, .F. ) ;
#17086 = FACE_OUTER_BOUND ( 'NONE', #15654, .T. ) ;
#17087 = ORIENTED_EDGE ( 'NONE', *, *, #3453, .T. ) ;
#17088 = CARTESIAN_POINT ( 'NONE',  ( -172.1050654871199868, 56.67212252599612299, -2.500000000000000000 ) ) ;
#17089 = VERTEX_POINT ( 'NONE', #4833 ) ;
#17090 = ORIENTED_EDGE ( 'NONE', *, *, #219, .F. ) ;
#17091 = CARTESIAN_POINT ( 'NONE',  ( -2.057045456857760524, -78.28153924966404986, -21.65063509461098690 ) ) ;
#17092 = ORIENTED_EDGE ( 'NONE', *, *, #13337, .T. ) ;
#17093 = DIRECTION ( 'NONE',  ( 0.000000000000000000, 0.000000000000000000, 1.000000000000000000 ) ) ;
#17094 = PRESENTATION_STYLE_ASSIGNMENT (( #8274 ) ) ;
#17095 = EDGE_CURVE ( 'NONE', #18001, #7282, #2984, .T. ) ;
#17096 = EDGE_CURVE ( 'NONE', #959, #6534, #5986, .T. ) ;
#17097 = DIRECTION ( 'NONE',  ( -0.1566598588826321192, 0.9876526153536342445, 7.798540720466730171E-17 ) ) ;
#17098 = ORIENTED_EDGE ( 'NONE', *, *, #12697, .T. ) ;
#17099 = EDGE_LOOP ( 'NONE', ( #7755, #16265 ) ) ;
#17100 = ORIENTED_EDGE ( 'NONE', *, *, #7149, .T. ) ;
#17101 = EDGE_CURVE ( 'NONE', #4996, #15703, #16219, .T. ) ;
#17102 = CARTESIAN_POINT ( 'NONE',  ( -48.80582637539254875, -22.92877817459017109, 8.660254037844417496 ) ) ;
#17103 = CYLINDRICAL_SURFACE ( 'NONE', #14545, 1.500000000000001554 ) ;
#17104 = CARTESIAN_POINT ( 'NONE',  ( -52.42732883989288695, -86.27119205267825919, 1.443110928631665584E-14 ) ) ;
#17105 = CARTESIAN_POINT ( 'NONE',  ( -3.538524379888211335, -78.51652903798800764, -4.330127018922185655 ) ) ;
#17106 = ORIENTED_EDGE ( 'NONE', *, *, #4726, .T. ) ;
#17107 = ORIENTED_EDGE ( 'NONE', *, *, #572, .T. ) ;
#17108 = ORIENTED_EDGE ( 'NONE', *, *, #8231, .T. ) ;
#17109 = ORIENTED_EDGE ( 'NONE', *, *, #10416, .F. ) ;
#17110 = FACE_OUTER_BOUND ( 'NONE', #3074, .T. ) ;
#17111 = EDGE_LOOP ( 'NONE', ( #5830, #14868 ) ) ;
#17112 = AXIS2_PLACEMENT_3D ( 'NONE', #4230, #17249, #18045 ) ;
#17113 = CARTESIAN_POINT ( 'NONE',  ( -6.995308533625909320, -79.06483854407721878, 21.65063509461100821 ) ) ;
#17114 = ORIENTED_EDGE ( 'NONE', *, *, #4948, .T. ) ;
#17115 = CYLINDRICAL_SURFACE ( 'NONE', #5401, 1.500000000000001554 ) ;
#17116 = FACE_OUTER_BOUND ( 'NONE', #10125, .T. ) ;
#17117 = ORIENTED_EDGE ( 'NONE', *, *, #11422, .T. ) ;
#17118 = EDGE_CURVE ( 'NONE', #8008, #2990, #15694, .T. ) ;
#17119 = LINE ( 'NONE', #6886, #8763 ) ;
#17120 = VECTOR ( 'NONE', #159, 1000.000000000000000 ) ;
#17121 = DIRECTION ( 'NONE',  ( -0.9876526153536336894, -0.1566598588826349503, 0.000000000000000000 ) ) ;
#17122 = ORIENTED_EDGE ( 'NONE', *, *, #3822, .F. ) ;
#17123 = DIRECTION ( 'NONE',  ( -0.1566598588826321192, 0.9876526153536342445, 7.798540720466730171E-17 ) ) ;
#17124 = CARTESIAN_POINT ( 'NONE',  ( -2.057045456857756971, -78.28153924966404986, 4.330127018922209636 ) ) ;
#17125 = VERTEX_POINT ( 'NONE', #8836 ) ;
#17126 = EDGE_LOOP ( 'NONE', ( #12873, #2066, #413, #3447 ) ) ;
#17127 = FACE_BOUND ( 'NONE', #7169, .T. ) ;
#17128 = DIRECTION ( 'NONE',  ( -0.1566598588826321747, 0.9876526153536343555, 0.000000000000000000 ) ) ;
#17129 = EDGE_CURVE ( 'NONE', #17592, #6604, #9112, .T. ) ;
#17130 = CARTESIAN_POINT ( 'NONE',  ( -15.88418207180859021, -80.47477727402089442, 8.660254037844412167 ) ) ;
#17131 = ORIENTED_EDGE ( 'NONE', *, *, #7403, .F. ) ;
#17132 = CARTESIAN_POINT ( 'NONE',  ( -9.464440072009985272, -79.45648819128378193, -17.32050807568878525 ) ) ;
#17133 = ORIENTED_EDGE ( 'NONE', *, *, #4493, .F. ) ;
#17134 = AXIS2_PLACEMENT_3D ( 'NONE', #14360, #14718, #7435 ) ;
#17135 = DIRECTION ( 'NONE',  ( -0.1566598588826321192, 0.9876526153536342445, 7.798540720466730171E-17 ) ) ;
#17136 = VERTEX_POINT ( 'NONE', #590 ) ;
#17137 = LINE ( 'NONE', #18773, #15157 ) ;
#17138 = DIRECTION ( 'NONE',  ( -0.9876526153536336894, -0.1566598588826349503, 0.000000000000000000 ) ) ;
#17139 = CARTESIAN_POINT ( 'NONE',  ( -81.73462711737164454, 33.01666666666666572, -24.99999999999999289 ) ) ;
#17140 = ORIENTED_EDGE ( 'NONE', *, *, #8606, .T. ) ;
#17141 = PRODUCT_DEFINITION_SHAPE ( 'NONE', 'NONE',  #18798 ) ;
#17142 = CIRCLE ( 'NONE', #14695, 12.74754878398196567 ) ;
#17143 = EDGE_CURVE ( 'NONE', #17712, #11092, #1775, .T. ) ;
#17144 = DIRECTION ( 'NONE',  ( 0.000000000000000000, 0.000000000000000000, -1.000000000000000000 ) ) ;
#17145 = CARTESIAN_POINT ( 'NONE',  ( -32.22008523532134205, -25.36048350923618955, -12.99038105676658006 ) ) ;
#17146 = DIRECTION ( 'NONE',  ( -0.1566598588826321192, 0.9876526153536342445, 7.798540720466731404E-17 ) ) ;
#17147 = DIRECTION ( 'NONE',  ( -0.000000000000000000, -0.000000000000000000, -1.000000000000000000 ) ) ;
#17148 = ORIENTED_EDGE ( 'NONE', *, *, #13198, .T. ) ;
#17149 = DIRECTION ( 'NONE',  ( 0.000000000000000000, 0.000000000000000000, 1.000000000000000000 ) ) ;
#17150 = AXIS2_PLACEMENT_3D ( 'NONE', #8804, #10212, #7395 ) ;
#17151 = CARTESIAN_POINT ( 'NONE',  ( -10.98555400521827963, -21.99229654325962002, -12.99038105676658006 ) ) ;
#17152 = ORIENTED_EDGE ( 'NONE', *, *, #7688, .F. ) ;
#17153 = EDGE_CURVE ( 'NONE', #16032, #15072, #11446, .T. ) ;
#17154 = DIRECTION ( 'NONE',  ( -1.000000000000000000, 0.000000000000000000, 0.000000000000000000 ) ) ;
#17155 = ORIENTED_EDGE ( 'NONE', *, *, #199, .F. ) ;
#17156 = EDGE_LOOP ( 'NONE', ( #14550, #7586, #15734, #13382 ) ) ;
#17157 = DIRECTION ( 'NONE',  ( -0.9876526153536344665, -0.1566598588826304539, 0.000000000000000000 ) ) ;
#17158 = EDGE_LOOP ( 'NONE', ( #17018, #2166 ) ) ;
#17159 = CARTESIAN_POINT ( 'NONE',  ( -89.99999999999998579, -35.00000000000001421, 100.5765140304660861 ) ) ;
#17160 = DIRECTION ( 'NONE',  ( -0.1566598588826321192, 0.9876526153536342445, 7.798540720466731404E-17 ) ) ;
#17161 = VECTOR ( 'NONE', #1497, 1000.000000000000000 ) ;
#17162 = DIRECTION ( 'NONE',  ( -0.1566598588826321192, 0.9876526153536342445, 7.798540720466730171E-17 ) ) ;
#17163 = CYLINDRICAL_SURFACE ( 'NONE', #2962, 1.500000000000001554 ) ;
#17164 = DIRECTION ( 'NONE',  ( -0.1566598588826321192, 0.9876526153536342445, 7.798540720466730171E-17 ) ) ;
#17165 = ORIENTED_EDGE ( 'NONE', *, *, #9393, .F. ) ;
#17166 = FACE_OUTER_BOUND ( 'NONE', #8108, .T. ) ;
#17167 = ADVANCED_FACE ( 'NONE', ( #10425 ), #17577, .F. ) ;
#17168 = EDGE_CURVE ( 'NONE', #9341, #14582, #3402, .T. ) ;
#17169 = LINE ( 'NONE', #8260, #16431 ) ;
#17170 = EDGE_CURVE ( 'NONE', #11831, #18705, #6186, .T. ) ;
#17171 = AXIS2_PLACEMENT_3D ( 'NONE', #2565, #12799, #11449 ) ;
#17172 = CARTESIAN_POINT ( 'NONE',  ( -306.1404785418517918, -2.850701963179328668, 9.951701414186818625E-16 ) ) ;
#17174 = ORIENTED_EDGE ( 'NONE', *, *, #3578, .F. ) ;
#17173 = CARTESIAN_POINT ( 'NONE',  ( 4.362696542940843081, -77.26325016692693737, 12.99038105676660493 ) ) ;
#17175 = EDGE_CURVE ( 'NONE', #3440, #13905, #4517, .T. ) ;
#17176 = VERTEX_POINT ( 'NONE', #8919 ) ;
#17177 = CARTESIAN_POINT ( 'NONE',  ( -38.10636591726526490, -83.99962409888010484, -4.330127018922185655 ) ) ;
#17178 = ORIENTED_EDGE ( 'NONE', *, *, #2080, .T. ) ;
#17179 = AXIS2_PLACEMENT_3D ( 'NONE', #17651, #7673, #13613 ) ;
#17180 = ORIENTED_EDGE ( 'NONE', *, *, #18125, .T. ) ;
#17181 = ORIENTED_EDGE ( 'NONE', *, *, #8245, .T. ) ;
#17182 = EDGE_LOOP ( 'NONE', ( #13113, #2860 ) ) ;
#17183 = CYLINDRICAL_SURFACE ( 'NONE', #16877, 1.500000000000001554 ) ;
#17184 = AXIS2_PLACEMENT_3D ( 'NONE', #9170, #9070, #447 ) ;
#17185 = DIRECTION ( 'NONE',  ( -0.9876526153536341335, -0.1566598588826327021, 0.000000000000000000 ) ) ;
#17186 = AXIS2_PLACEMENT_3D ( 'NONE', #10225, #3028, #7406 ) ;
#17187 = DIRECTION ( 'NONE',  ( 0.000000000000000000, 0.000000000000000000, 1.000000000000000000 ) ) ;
#17188 = CIRCLE ( 'NONE', #7188, 1.500000000000000000 ) ;
#17189 =( GEOMETRIC_REPRESENTATION_CONTEXT ( 3 ) GLOBAL_UNCERTAINTY_ASSIGNED_CONTEXT ( ( #18578 ) ) GLOBAL_UNIT_ASSIGNED_CONTEXT ( ( #10098, #17244, #8773 ) ) REPRESENTATION_CONTEXT ( 'NONE', 'WORKASPACE' ) );
#17190 = DIRECTION ( 'NONE',  ( -0.1566598588826321192, 0.9876526153536342445, 7.798540720466731404E-17 ) ) ;
#17191 = VERTEX_POINT ( 'NONE', #17855 ) ;
#17193 = EDGE_LOOP ( 'NONE', ( #11788, #13597 ) ) ;
#17192 = CIRCLE ( 'NONE', #11403, 150.0000000000000284 ) ;
#17194 = EDGE_CURVE ( 'NONE', #4463, #2115, #11917, .T. ) ;
#17195 = EDGE_LOOP ( 'NONE', ( #8785, #11117, #3712, #3598 ) ) ;
#17196 = CARTESIAN_POINT ( 'NONE',  ( -33.20773785067495254, -25.51714336811882688, -17.32050807568878170 ) ) ;
#17197 = CARTESIAN_POINT ( 'NONE',  ( -37.94164760650263446, -21.20551972688122433, 12.99038105676661736 ) ) ;
#17198 = CARTESIAN_POINT ( 'NONE',  ( -49.01017969633301163, -28.02370111024092481, 12.99038105676661736 ) ) ;
#17199 = DIRECTION ( 'NONE',  ( -0.1566598588826321192, 0.9876526153536342445, 7.798540720466730171E-17 ) ) ;
#17200 = DIRECTION ( 'NONE',  ( -0.9876526153536341335, -0.1566598588826327021, 0.000000000000000000 ) ) ;
#17201 = ORIENTED_EDGE ( 'NONE', *, *, #12497, .T. ) ;
#17202 = EDGE_CURVE ( 'NONE', #10018, #4398, #14515, .T. ) ;
#17203 = ORIENTED_EDGE ( 'NONE', *, *, #7428, .T. ) ;
#17204 = ORIENTED_EDGE ( 'NONE', *, *, #11491, .T. ) ;
#17205 = VERTEX_POINT ( 'NONE', #10622 ) ;
#17206 = DIRECTION ( 'NONE',  ( -0.1566598588826321192, 0.9876526153536342445, 7.798540720466730171E-17 ) ) ;
#17207 = EDGE_CURVE ( 'NONE', #7553, #15083, #13586, .T. ) ;
#17208 = ORIENTED_EDGE ( 'NONE', *, *, #81, .F. ) ;
#17209 = FACE_BOUND ( 'NONE', #4747, .T. ) ;
#17210 = VECTOR ( 'NONE', #8285, 1000.000000000000000 ) ;
#17211 = FACE_OUTER_BOUND ( 'NONE', #7972, .T. ) ;
#17212 = VERTEX_POINT ( 'NONE', #18258 ) ;
#17213 = CARTESIAN_POINT ( 'NONE',  ( -22.63303206852135929, -18.77729191420043620, 8.660254037844417496 ) ) ;
#17214 = CARTESIAN_POINT ( 'NONE',  ( -50.45202360918563045, -85.95787233491300583, 8.660254037844412167 ) ) ;
#17215 = DIRECTION ( 'NONE',  ( -0.1566598588826321192, 0.9876526153536342445, 7.798540720466730171E-17 ) ) ;
#17216 = APPLICATION_PROTOCOL_DEFINITION ( 'draft international standard', 'automotive_design', 1998, #5926 ) ;
#17217 = AXIS2_PLACEMENT_3D ( 'NONE', #17424, #1316, #1492 ) ;
#17218 = DIRECTION ( 'NONE',  ( 0.000000000000000000, 0.000000000000000000, 1.000000000000000000 ) ) ;
#17219 = CARTESIAN_POINT ( 'NONE',  ( -59.79999999999999716, 0.000000000000000000, -25.00000000000000000 ) ) ;
#17220 = DIRECTION ( 'NONE',  ( 0.000000000000000000, -1.000000000000000000, 0.000000000000000000 ) ) ;
#17221 = CIRCLE ( 'NONE', #5392, 2.000000000000001776 ) ;
#17222 = DIRECTION ( 'NONE',  ( -0.9876526153536336894, -0.1566598588826349503, 0.000000000000000000 ) ) ;
#17223 = PLANE ( 'NONE',  #4405 ) ;
#17224 = VERTEX_POINT ( 'NONE', #12302 ) ;
#17225 = ORIENTED_EDGE ( 'NONE', *, *, #11457, .T. ) ;
#17226 = FACE_BOUND ( 'NONE', #17743, .T. ) ;
#17227 = DIRECTION ( 'NONE',  ( -0.1566598588826321192, 0.9876526153536342445, 7.798540720466731404E-17 ) ) ;
#17228 = ORIENTED_EDGE ( 'NONE', *, *, #3564, .F. ) ;
#17229 = EDGE_CURVE ( 'NONE', #17593, #4102, #9289, .T. ) ;
#17230 = DIRECTION ( 'NONE',  ( -0.1566598588826321192, 0.9876526153536342445, 7.798540720466730171E-17 ) ) ;
#17231 = CARTESIAN_POINT ( 'NONE',  ( -27.28182215855319015, -24.57718421482303484, 21.65063509461101887 ) ) ;
#17232 = VECTOR ( 'NONE', #1390, 1000.000000000000000 ) ;
#17233 = EDGE_LOOP ( 'NONE', ( #6166, #13118 ) ) ;
#17234 = DIRECTION ( 'NONE',  ( -0.9876526153536336894, -0.1566598588826349503, 0.000000000000000000 ) ) ;
#17235 = VECTOR ( 'NONE', #5737, 1000.000000000000114 ) ;
#17236 = EDGE_CURVE ( 'NONE', #7437, #6198, #12206, .T. ) ;
#17237 = AXIS2_PLACEMENT_3D ( 'NONE', #1926, #16516, #3508 ) ;
#17238 = DIRECTION ( 'NONE',  ( -0.9876526153536336894, -0.1566598588826350336, 0.000000000000000000 ) ) ;
#17239 = LINE ( 'NONE', #4217, #12718 ) ;
#17240 = VECTOR ( 'NONE', #10752, 1000.000000000000000 ) ;
#17241 = DIRECTION ( 'NONE',  ( -0.1566598588826321192, 0.9876526153536342445, 7.798540720466731404E-17 ) ) ;
#17242 = DIRECTION ( 'NONE',  ( -0.1566598588826321747, 0.9876526153536343555, 0.000000000000000000 ) ) ;
#17243 = CARTESIAN_POINT ( 'NONE',  ( -11.93357161039406300, -79.84813783849037350, 12.99038105676661203 ) ) ;
#17244 =( NAMED_UNIT ( * ) PLANE_ANGLE_UNIT ( ) SI_UNIT ( $, .RADIAN. ) );
#17245 = VERTEX_POINT ( 'NONE', #8265 ) ;
#17246 = CARTESIAN_POINT ( 'NONE',  ( -12.92122422574768592, -80.00479769737299307, 17.32050807568881368 ) ) ;
#17247 = ORIENTED_EDGE ( 'NONE', *, *, #14245, .T. ) ;
#17248 = CARTESIAN_POINT ( 'NONE',  ( -13.41505053342451426, -80.08312762681433128, 12.99038105676661203 ) ) ;
#17249 = DIRECTION ( 'NONE',  ( -0.1566598588826321747, 0.9876526153536343555, 0.000000000000000000 ) ) ;
#17250 = AXIS2_PLACEMENT_3D ( 'NONE', #9673, #16987, #1069 ) ;
#17251 = CARTESIAN_POINT ( 'NONE',  ( -31.68662391746665463, -82.98133501614300656, 12.99038105676661203 ) ) ;
#17252 = VERTEX_POINT ( 'NONE', #18048 ) ;
#17253 = DIRECTION ( 'NONE',  ( -0.9876526153536336894, -0.1566598588826349503, 0.000000000000000000 ) ) ;
#17254 = AXIS2_PLACEMENT_3D ( 'NONE', #7315, #14499, #13067 ) ;
#17255 = ORIENTED_EDGE ( 'NONE', *, *, #15024, .F. ) ;
#17256 = DIRECTION ( 'NONE',  ( -0.1566598588826321747, 0.9876526153536343555, 0.000000000000000000 ) ) ;
#17258 = ORIENTED_EDGE ( 'NONE', *, *, #8750, .F. ) ;
#17257 = DIRECTION ( 'NONE',  ( -0.9876526153536336894, -0.1566598588826349503, 0.000000000000000000 ) ) ;
#17259 = DIRECTION ( 'NONE',  ( -0.9876526153536341335, -0.1566598588826327021, 0.000000000000000000 ) ) ;
#17260 = ORIENTED_EDGE ( 'NONE', *, *, #13694, .T. ) ;
#17261 = ORIENTED_EDGE ( 'NONE', *, *, #4578, .F. ) ;
#17262 = EDGE_LOOP ( 'NONE', ( #18571, #9394 ) ) ;
#17263 = AXIS2_PLACEMENT_3D ( 'NONE', #6171, #9187, #852 ) ;
#17264 = ADVANCED_FACE ( 'NONE', ( #12117 ), #14028, .F. ) ;
#17265 = CIRCLE ( 'NONE', #11746, 1.500000000000001332 ) ;
#17266 = CARTESIAN_POINT ( 'NONE',  ( -36.62488699423479943, -83.76463431055617548, 12.99038105676661203 ) ) ;
#17267 = CARTESIAN_POINT ( 'NONE',  ( -42.09661138885763165, -26.92708209806250608, 21.65063509461101887 ) ) ;
#17268 = CIRCLE ( 'NONE', #15716, 1.499999999999999556 ) ;
#17269 = DIRECTION ( 'NONE',  ( -0.000000000000000000, -0.000000000000000000, -1.000000000000000000 ) ) ;
#17270 = AXIS2_PLACEMENT_3D ( 'NONE', #8158, #3583, #8051 ) ;
#17271 = VECTOR ( 'NONE', #12514, 1000.000000000000000 ) ;
#17272 = FACE_OUTER_BOUND ( 'NONE', #14801, .T. ) ;
#17273 = CARTESIAN_POINT ( 'NONE',  ( -27.57129514528951120, -19.56059120861359801, 17.32050807568881723 ) ) ;
#17274 = EDGE_CURVE ( 'NONE', #3175, #8612, #16599, .T. ) ;
#17275 = CARTESIAN_POINT ( 'NONE',  ( -79.91688375903190433, -27.86356372939305714, -17.32050807568878170 ) ) ;
#17276 = ADVANCED_FACE ( 'NONE', ( #9484 ), #13642, .F. ) ;
#17277 = CARTESIAN_POINT ( 'NONE',  ( -170.3665179301995352, 31.30647307655612366, 9.951701414186830458E-16 ) ) ;
#17278 = CIRCLE ( 'NONE', #17581, 1.500000000000000000 ) ;
#17279 = FACE_BOUND ( 'NONE', #16779, .T. ) ;
#17280 = ORIENTED_EDGE ( 'NONE', *, *, #3058, .F. ) ;
#17281 = VECTOR ( 'NONE', #12318, 1000.000000000000000 ) ;
#17282 = VERTEX_POINT ( 'NONE', #15069 ) ;
#17283 = AXIS2_PLACEMENT_3D ( 'NONE', #14161, #18481, #6594 ) ;
#17284 = ORIENTED_EDGE ( 'NONE', *, *, #13193, .T. ) ;
#17285 = CARTESIAN_POINT ( 'NONE',  ( -61.31620237807555895, -87.68113078262193483, -21.65063509461098690 ) ) ;
#17286 = VERTEX_POINT ( 'NONE', #10888 ) ;
#17287 = EDGE_LOOP ( 'NONE', ( #2173, #14573 ) ) ;
#17288 = FACE_OUTER_BOUND ( 'NONE', #17933, .T. ) ;
#17289 = FACE_BOUND ( 'NONE', #5389, .T. ) ;
#17290 = CIRCLE ( 'NONE', #18, 1.500000000000000444 ) ;
#17291 = EDGE_CURVE ( 'NONE', #9121, #10521, #17959, .T. ) ;
#17292 = EDGE_CURVE ( 'NONE', #12642, #2898, #2092, .T. ) ;
#17293 = AXIS2_PLACEMENT_3D ( 'NONE', #16872, #18615, #14093 ) ;
#17294 = ORIENTED_EDGE ( 'NONE', *, *, #12961, .F. ) ;
#17295 = CARTESIAN_POINT ( 'NONE',  ( 5.481473465377026955, -12.88229205725314763, 25.00000000000000000 ) ) ;
#17296 = ADVANCED_FACE ( 'NONE', ( #15171, #5006 ), #16501, .F. ) ;
#17297 = VECTOR ( 'NONE', #13286, 1000.000000000000000 ) ;
#17298 = VECTOR ( 'NONE', #18131, 1000.000000000000000 ) ;
#17299 = CARTESIAN_POINT ( 'NONE',  ( -94.14047854185179176, 6.938893903907228378E-15, -2.500000000000000000 ) ) ;
#17300 = DIRECTION ( 'NONE',  ( -0.1566598588826321747, 0.9876526153536343555, 0.000000000000000000 ) ) ;
#17301 = DIRECTION ( 'NONE',  ( 0.000000000000000000, 0.000000000000000000, 1.000000000000000000 ) ) ;
#17302 = AXIS2_PLACEMENT_3D ( 'NONE', #16076, #4595, #11675 ) ;
#17303 = CARTESIAN_POINT ( 'NONE',  ( -71.90911978745813826, 1.387778780781445676E-14, 20.00000000000001421 ) ) ;
#17304 = VECTOR ( 'NONE', #12938, 1000.000000000000000 ) ;
#17305 = ORIENTED_EDGE ( 'NONE', *, *, #10238, .T. ) ;
#17306 = ORIENTED_EDGE ( 'NONE', *, *, #5862, .F. ) ;
#17307 = ORIENTED_EDGE ( 'NONE', *, *, #14697, .T. ) ;
#17308 = EDGE_LOOP ( 'NONE', ( #17582, #15305 ) ) ;
#17309 = CARTESIAN_POINT ( 'NONE',  ( -78.43540483600145308, -27.62857394106912068, 8.660254037844417496 ) ) ;
#17310 = ORIENTED_EDGE ( 'NONE', *, *, #2006, .F. ) ;
#17311 = CIRCLE ( 'NONE', #9102, 1.499999999999999556 ) ;
#17312 = FACE_BOUND ( 'NONE', #15505, .T. ) ;
#17313 = CIRCLE ( 'NONE', #17004, 1.500000000000001332 ) ;
#17314 = DIRECTION ( 'NONE',  ( -0.1566598588826321747, 0.9876526153536343555, 0.000000000000000000 ) ) ;
#17315 = ADVANCED_FACE ( 'NONE', ( #3587 ), #9576, .F. ) ;
#17316 = ORIENTED_EDGE ( 'NONE', *, *, #18576, .F. ) ;
#17317 = CIRCLE ( 'NONE', #12115, 1.500000000000000888 ) ;
#17318 = DIRECTION ( 'NONE',  ( -0.1566598588826321747, 0.9876526153536343555, 0.000000000000000000 ) ) ;
#17319 = CARTESIAN_POINT ( 'NONE',  ( -71.02801022084922522, -26.45362499944937085, -21.65063509461097979 ) ) ;
#17320 = ADVANCED_FACE ( 'NONE', ( #2272 ), #8054, .F. ) ;
#17321 = CIRCLE ( 'NONE', #6416, 145.0000000000000284 ) ;
#17322 = CARTESIAN_POINT ( 'NONE',  ( -43.08426400421126345, -27.08374195694514341, -17.32050807568878170 ) ) ;
#17323 = LINE ( 'NONE', #1384, #16895 ) ;
#17324 = AXIS2_PLACEMENT_3D ( 'NONE', #6785, #6873, #11201 ) ;
#17325 = DIRECTION ( 'NONE',  ( 2.671473304378624222E-16, 0.000000000000000000, 1.000000000000000000 ) ) ;
#17326 = ORIENTED_EDGE ( 'NONE', *, *, #5478, .T. ) ;
#17327 = ORIENTED_EDGE ( 'NONE', *, *, #7361, .F. ) ;
#17328 = DIRECTION ( 'NONE',  ( 1.000000000000000000, 0.000000000000000000, 0.000000000000000000 ) ) ;
#17329 = CIRCLE ( 'NONE', #17626, 1.500000000000000888 ) ;
#17330 = CARTESIAN_POINT ( 'NONE',  ( 0.000000000000000000, 0.000000000000000000, 35.00000000000000000 ) ) ;
#17331 = CIRCLE ( 'NONE', #979, 1.500000000000000888 ) ;
#17332 = CARTESIAN_POINT ( 'NONE',  ( -28.06512145296634486, -19.63892113805489714, -12.99038105676658006 ) ) ;
#17333 = EDGE_LOOP ( 'NONE', ( #11962, #6015 ) ) ;
#17334 = CYLINDRICAL_SURFACE ( 'NONE', #1259, 1.500000000000001554 ) ;
#17335 = VECTOR ( 'NONE', #969, 1000.000000000000000 ) ;
#17336 = CARTESIAN_POINT ( 'NONE',  ( -74.48479437458692587, -27.00193450553859620, 4.330127018922218518 ) ) ;
#17337 = CARTESIAN_POINT ( 'NONE',  ( -48.02252708097942246, -27.86704125135829813, -17.32050807568878170 ) ) ;
#17338 = CARTESIAN_POINT ( 'NONE',  ( -69.99999999999998579, -45.00000000000000711, -25.00000000000000000 ) ) ;
#17339 = FACE_OUTER_BOUND ( 'NONE', #8544, .T. ) ;
#17340 = EDGE_CURVE ( 'NONE', #949, #12885, #12506, .T. ) ;
#17341 = EDGE_CURVE ( 'NONE', #17772, #9210, #17265, .T. ) ;
#17342 = CARTESIAN_POINT ( 'NONE',  ( -39.62747985047356281, -26.53543245085591806, 8.660254037844417496 ) ) ;
#17343 = VERTEX_POINT ( 'NONE', #3491 ) ;
#17344 = DIRECTION ( 'NONE',  ( 0.000000000000000000, 0.000000000000000000, 1.000000000000000000 ) ) ;
#17345 = DIRECTION ( 'NONE',  ( -0.9876526153536341335, -0.1566598588826327021, 0.000000000000000000 ) ) ;
#17346 = DIRECTION ( 'NONE',  ( -0.1566598588826321192, 0.9876526153536342445, 7.798540720466731404E-17 ) ) ;
#17347 = CIRCLE ( 'NONE', #2492, 15.83618137761393463 ) ;
#17348 = DIRECTION ( 'NONE',  ( -0.1566598588826321747, 0.9876526153536343555, 0.000000000000000000 ) ) ;
#17349 = EDGE_CURVE ( 'NONE', #3641, #2692, #5748, .T. ) ;
#17351 = ORIENTED_EDGE ( 'NONE', *, *, #11353, .F. ) ;
#17350 = DIRECTION ( 'NONE',  ( -0.9876526153536336894, -0.1566598588826349503, 0.000000000000000000 ) ) ;
#17352 = CARTESIAN_POINT ( 'NONE',  ( -20.32861884089991023, -81.17974663899272514, -12.99038105676658539 ) ) ;
#17353 = VERTEX_POINT ( 'NONE', #10703 ) ;
#17354 = AXIS2_PLACEMENT_3D ( 'NONE', #2648, #18634, #11350 ) ;
#17355 = ORIENTED_EDGE ( 'NONE', *, *, #13765, .F. ) ;
#17356 = LINE ( 'NONE', #7028, #2773 ) ;
#17357 = DIRECTION ( 'NONE',  ( -0.9876526153536341335, -0.1566598588826327021, 0.000000000000000000 ) ) ;
#17358 = VECTOR ( 'NONE', #14415, 1000.000000000000000 ) ;
#17359 = DIRECTION ( 'NONE',  ( 1.000000000000000000, 0.000000000000000000, -2.631994239413086031E-16 ) ) ;
#17360 = ORIENTED_EDGE ( 'NONE', *, *, #15152, .F. ) ;
#17361 = LINE ( 'NONE', #8798, #13356 ) ;
#17362 = CARTESIAN_POINT ( 'NONE',  ( -48.97054468615519340, -85.72288254658904805, -8.660254037844385522 ) ) ;
#17363 = CARTESIAN_POINT ( 'NONE',  ( -22.79775037928398618, -81.57139628619930249, 1.443110928631665584E-14 ) ) ;
#17364 = DIRECTION ( 'NONE',  ( -0.1566598588826321192, 0.9876526153536342445, 7.798540720466730171E-17 ) ) ;
#17365 = FACE_BOUND ( 'NONE', #8851, .T. ) ;
#17366 = DIRECTION ( 'NONE',  ( 8.693966348389027220E-17, -1.991237296706374949E-16, 1.000000000000000000 ) ) ;
#17367 = CARTESIAN_POINT ( 'NONE',  ( -67.77557938805200877, -31.00023842901093118, 1.869203119972154228E-14 ) ) ;
#17368 = EDGE_LOOP ( 'NONE', ( #5730, #12668 ) ) ;
#17369 = EDGE_CURVE ( 'NONE', #12390, #13736, #15114, .T. ) ;
#17370 = VERTEX_POINT ( 'NONE', #2477 ) ;
#17371 = ORIENTED_EDGE ( 'NONE', *, *, #17369, .T. ) ;
#17372 = CARTESIAN_POINT ( 'NONE',  ( 5.481473465377021625, 12.88229205725314763, 25.00000000000000000 ) ) ;
#17373 = AXIS2_PLACEMENT_3D ( 'NONE', #16692, #12397, #15158 ) ;
#17374 = ORIENTED_EDGE ( 'NONE', *, *, #13083, .T. ) ;
#17375 = ORIENTED_EDGE ( 'NONE', *, *, #18277, .F. ) ;
#17376 = ADVANCED_FACE ( 'NONE', ( #4923 ), #11, .F. ) ;
#17377 = DIRECTION ( 'NONE',  ( -0.1566598588826321192, 0.9876526153536342445, 7.798540720466730171E-17 ) ) ;
#17378 = VERTEX_POINT ( 'NONE', #4158 ) ;
#17379 = CARTESIAN_POINT ( 'NONE',  ( -174.0670050711101737, 56.28339404658827760, 2.500000000000000000 ) ) ;
#17380 = FACE_BOUND ( 'NONE', #10092, .T. ) ;
#17381 = CARTESIAN_POINT ( 'NONE',  ( -56.21322099054476240, -24.10372711620991382, 21.65063509461102242 ) ) ;
#17382 = DIRECTION ( 'NONE',  ( -0.9876526153536336894, -0.1566598588826349503, 0.000000000000000000 ) ) ;
#17383 = ORIENTED_EDGE ( 'NONE', *, *, #16497, .T. ) ;
#17384 = FACE_BOUND ( 'NONE', #5347, .T. ) ;
#17385 = ORIENTED_EDGE ( 'NONE', *, *, #3694, .T. ) ;
#17386 = DIRECTION ( 'NONE',  ( -0.1566598588826321192, 0.9876526153536342445, 7.798540720466731404E-17 ) ) ;
#17387 = EDGE_CURVE ( 'NONE', #11671, #5804, #2395, .T. ) ;
#17388 = CARTESIAN_POINT ( 'NONE',  ( -50.49165861936346289, -28.25869089856487903, 12.99038105676661736 ) ) ;
#17389 = LINE ( 'NONE', #7238, #9081 ) ;
#17390 = FACE_BOUND ( 'NONE', #6627, .T. ) ;
#17391 = LINE ( 'NONE', #2778, #11154 ) ;
#17392 = ADVANCED_FACE ( 'NONE', ( #1351 ), #15737, .F. ) ;
#17393 = ORIENTED_EDGE ( 'NONE', *, *, #11070, .F. ) ;
#17394 = EDGE_LOOP ( 'NONE', ( #5342, #4000, #18500, #6681 ) ) ;
#17395 = ADVANCED_FACE ( 'NONE', ( #7130 ), #2921, .F. ) ;
#17396 = ORIENTED_EDGE ( 'NONE', *, *, #4474, .F. ) ;
#17397 = ORIENTED_EDGE ( 'NONE', *, *, #14368, .F. ) ;
#17398 = DIRECTION ( 'NONE',  ( -0.000000000000000000, -0.000000000000000000, -1.000000000000000000 ) ) ;
#17399 = ORIENTED_EDGE ( 'NONE', *, *, #12615, .F. ) ;
#17400 = DIRECTION ( 'NONE',  ( 1.000000000000000000, 0.000000000000000000, 0.000000000000000000 ) ) ;
#17401 = DIRECTION ( 'NONE',  ( -0.1566598588826321192, 0.9876526153536342445, 7.798540720466730171E-17 ) ) ;
#17402 = EDGE_LOOP ( 'NONE', ( #17307, #8746, #7298, #2097, #15325 ) ) ;
#17403 = DIRECTION ( 'NONE',  ( -0.1566598588826321192, 0.9876526153536342445, 7.798540720466731404E-17 ) ) ;
#17404 = PRODUCT_CONTEXT ( 'NONE', #364, 'mechanical' ) ;
#17405 = DIRECTION ( 'NONE',  ( -0.9876526153536341335, -0.1566598588826327021, 0.000000000000000000 ) ) ;
#17406 = DIRECTION ( 'NONE',  ( -0.1566598588826321192, 0.9876526153536342445, 7.798540720466731404E-17 ) ) ;
#17407 = ADVANCED_FACE ( 'NONE', ( #15545 ), #8549, .F. ) ;
#17408 = DIRECTION ( 'NONE',  ( -0.1566598588826321192, 0.9876526153536342445, 7.798540720466731404E-17 ) ) ;
#17409 = EDGE_CURVE ( 'NONE', #12460, #5191, #12875, .T. ) ;
#17410 = ORIENTED_EDGE ( 'NONE', *, *, #18468, .T. ) ;
#17411 = EDGE_LOOP ( 'NONE', ( #15428, #4397, #7071, #13881 ) ) ;
#17412 = DIRECTION ( 'NONE',  ( -0.1566598588826321192, 0.9876526153536342445, 7.798540720466730171E-17 ) ) ;
#17413 = ADVANCED_FACE ( 'NONE', ( #4265 ), #5701, .F. ) ;
#17414 = LINE ( 'NONE', #16161, #4757 ) ;
#17415 = DIRECTION ( 'NONE',  ( -0.9868632313631133801, 0.1615579233078772436, -0.000000000000000000 ) ) ;
#17416 = ORIENTED_EDGE ( 'NONE', *, *, #4137, .T. ) ;
#17417 = EDGE_CURVE ( 'NONE', #3263, #14051, #10846, .T. ) ;
#17418 = ORIENTED_EDGE ( 'NONE', *, *, #14706, .T. ) ;
#17419 = VERTEX_POINT ( 'NONE', #18639 ) ;
#17420 = DIRECTION ( 'NONE',  ( -0.1566598588826321192, 0.9876526153536342445, 7.798540720466730171E-17 ) ) ;
#17421 = DIRECTION ( 'NONE',  ( -0.9876526153536341335, -0.1566598588826330907, 0.000000000000000000 ) ) ;
#17422 = AXIS2_PLACEMENT_3D ( 'NONE', #875, #7967, #11324 ) ;
#17423 = CARTESIAN_POINT ( 'NONE',  ( -70.00000000000000000, 44.99999999999999289, -19.99999999999998934 ) ) ;
#17424 = CARTESIAN_POINT ( 'NONE',  ( 0.000000000000000000, 0.000000000000000000, 30.00000000000000000 ) ) ;
#17425 = CARTESIAN_POINT ( 'NONE',  ( -29.25712738926042888, -24.89050393258829175, -21.65063509461098334 ) ) ;
#17426 = CARTESIAN_POINT ( 'NONE',  ( -14.93616446663280328, -22.61893597879013740, -8.660254037844380193 ) ) ;
#17427 = CYLINDRICAL_SURFACE ( 'NONE', #9537, 1.500000000000001554 ) ;
#17428 = DIRECTION ( 'NONE',  ( 0.000000000000000000, 0.000000000000000000, 1.000000000000000000 ) ) ;
#17429 = EDGE_LOOP ( 'NONE', ( #2572, #14255, #1980, #17973 ) ) ;
#17430 = DIRECTION ( 'NONE',  ( -0.1566598588826321192, 0.9876526153536342445, 7.798540720466730171E-17 ) ) ;
#17432 = ORIENTED_EDGE ( 'NONE', *, *, #6987, .F. ) ;
#17431 = DIRECTION ( 'NONE',  ( -0.1566598588826321747, 0.9876526153536343555, 0.000000000000000000 ) ) ;
#17433 = AXIS2_PLACEMENT_3D ( 'NONE', #2229, #16544, #3534 ) ;
#17434 = CYLINDRICAL_SURFACE ( 'NONE', #8787, 1.500000000000001554 ) ;
#17435 = EDGE_LOOP ( 'NONE', ( #5267, #5063, #9488, #17832 ) ) ;
#17436 = EDGE_CURVE ( 'NONE', #9991, #3282, #8718, .T. ) ;
#17437 = EDGE_CURVE ( 'NONE', #795, #11890, #11356, .T. ) ;
#17438 = DIRECTION ( 'NONE',  ( -0.9876526153536336894, -0.1566598588826349503, 0.000000000000000000 ) ) ;
#17439 = CARTESIAN_POINT ( 'NONE',  ( 0.000000000000000000, 0.000000000000000000, -22.00000000000000711 ) ) ;
#17440 = LINE ( 'NONE', #4425, #2528 ) ;
#17441 = ORIENTED_EDGE ( 'NONE', *, *, #16728, .T. ) ;
#17442 = DIRECTION ( 'NONE',  ( 0.000000000000000000, 0.000000000000000000, 1.000000000000000000 ) ) ;
#17443 = DIRECTION ( 'NONE',  ( 0.000000000000000000, 0.000000000000000000, 1.000000000000000000 ) ) ;
#17444 = DIRECTION ( 'NONE',  ( -0.1566598588826321192, 0.9876526153536342445, 7.798540720466731404E-17 ) ) ;
#17445 = AXIS2_PLACEMENT_3D ( 'NONE', #14165, #11114, #11304 ) ;
#17446 = LINE ( 'NONE', #4431, #4107 ) ;
#17447 = FACE_BOUND ( 'NONE', #2925, .T. ) ;
#17448 = DIRECTION ( 'NONE',  ( -0.1566598588826321747, 0.9876526153536343555, 0.000000000000000000 ) ) ;
#17449 = DIRECTION ( 'NONE',  ( -0.000000000000000000, -0.000000000000000000, -1.000000000000000000 ) ) ;
#17450 = ORIENTED_EDGE ( 'NONE', *, *, #16806, .F. ) ;
#17451 = VERTEX_POINT ( 'NONE', #17372 ) ;
#17452 = DIRECTION ( 'NONE',  ( -0.9201637183752249260, -0.3915338189555018777, -3.511704013281690003E-17 ) ) ;
#17453 = VERTEX_POINT ( 'NONE', #14503 ) ;
#17454 = AXIS2_PLACEMENT_3D ( 'NONE', #17172, #4153, #9940 ) ;
#17455 = ORIENTED_EDGE ( 'NONE', *, *, #4749, .T. ) ;
#17456 = VERTEX_POINT ( 'NONE', #1435 ) ;
#17457 = DIRECTION ( 'NONE',  ( -0.9876526153536341335, -0.1566598588826327021, 0.000000000000000000 ) ) ;
#17458 = CIRCLE ( 'NONE', #16220, 2.000000000000001776 ) ;
#17459 = FACE_BOUND ( 'NONE', #4497, .T. ) ;
#17460 = EDGE_CURVE ( 'NONE', #1264, #14170, #7225, .T. ) ;
#17461 = CARTESIAN_POINT ( 'NONE',  ( -36.46016868347218320, -20.97052993855727010, -4.330127018922180326 ) ) ;
#17462 = AXIS2_PLACEMENT_3D ( 'NONE', #7420, #7790, #10431 ) ;
#17463 = DIRECTION ( 'NONE',  ( -0.1566598588826321192, 0.9876526153536342445, 7.798540720466730171E-17 ) ) ;
#17464 = ORIENTED_EDGE ( 'NONE', *, *, #15184, .F. ) ;
#17465 = EDGE_CURVE ( 'NONE', #3229, #9249, #6360, .T. ) ;
#17466 = FACE_BOUND ( 'NONE', #17193, .T. ) ;
#17467 = ORIENTED_EDGE ( 'NONE', *, *, #10214, .T. ) ;
#17468 = DIRECTION ( 'NONE',  ( 0.000000000000000000, 0.000000000000000000, 1.000000000000000000 ) ) ;
#17469 = CARTESIAN_POINT ( 'NONE',  ( -63.62061560569699736, -25.27867605782964944, 17.32050807568882078 ) ) ;
#17470 = CIRCLE ( 'NONE', #8677, 1.499999999999999556 ) ;
#17471 = DIRECTION ( 'NONE',  ( -0.1566598588826321192, 0.9876526153536342445, 7.798540720466731404E-17 ) ) ;
#17472 = CARTESIAN_POINT ( 'NONE',  ( -52.26261052913024230, -23.47708768067938934, 17.32050807568881723 ) ) ;
#17473 = DIRECTION ( 'NONE',  ( -0.1566598588826321747, 0.9876526153536343555, 0.000000000000000000 ) ) ;
#17474 = ORIENTED_EDGE ( 'NONE', *, *, #12840, .T. ) ;
#17475 = EDGE_LOOP ( 'NONE', ( #7699, #8548, #5903, #6514, #11004 ) ) ;
#17476 = ORIENTED_EDGE ( 'NONE', *, *, #15510, .T. ) ;
#17477 = ORIENTED_EDGE ( 'NONE', *, *, #315, .T. ) ;
#17478 = FACE_OUTER_BOUND ( 'NONE', #2988, .T. ) ;
#17479 = CIRCLE ( 'NONE', #18729, 1.500000000000000888 ) ;
#17480 = ORIENTED_EDGE ( 'NONE', *, *, #10634, .F. ) ;
#17481 = FACE_BOUND ( 'NONE', #4378, .T. ) ;
#17482 = CARTESIAN_POINT ( 'NONE',  ( -105.9742111339482307, -32.54855632894931716, -2.500000000000000000 ) ) ;
#17483 = ORIENTED_EDGE ( 'NONE', *, *, #15389, .F. ) ;
#17484 = EDGE_CURVE ( 'NONE', #1263, #755, #2703, .T. ) ;
#17485 = AXIS2_PLACEMENT_3D ( 'NONE', #4601, #1757, #17997 ) ;
#17486 = ORIENTED_EDGE ( 'NONE', *, *, #242, .T. ) ;
#17487 = AXIS2_PLACEMENT_3D ( 'NONE', #3565, #16484, #8030 ) ;
#17488 = ORIENTED_EDGE ( 'NONE', *, *, #8928, .F. ) ;
#17489 = CARTESIAN_POINT ( 'NONE',  ( -40.41077914488671041, -21.59716937408780524, 17.32050807568881723 ) ) ;
#17490 = ADVANCED_FACE ( 'NONE', ( #12683 ), #12585, .F. ) ;
#17491 = FACE_BOUND ( 'NONE', #6636, .T. ) ;
#17492 = AXIS2_PLACEMENT_3D ( 'NONE', #11512, #17346, #17428 ) ;
#17493 = DIRECTION ( 'NONE',  ( 0.000000000000000000, 0.000000000000000000, 1.000000000000000000 ) ) ;
#17494 = FACE_OUTER_BOUND ( 'NONE', #2764, .T. ) ;
#17495 = CARTESIAN_POINT ( 'NONE',  ( -84.20693962813486166, 32.64562644091790844, 30.00000000000002842 ) ) ;
#17496 = CARTESIAN_POINT ( 'NONE',  ( -174.6909448281246569, 55.69916092364878324, -4.223374618371431133 ) ) ;
#17497 = CARTESIAN_POINT ( 'NONE',  ( -9.464440072009985272, -79.45648819128378193, 1.424741226644455312E-14 ) ) ;
#17498 = DIRECTION ( 'NONE',  ( -0.1566598588826321192, 0.9876526153536342445, 7.798540720466730171E-17 ) ) ;
#17499 = EDGE_LOOP ( 'NONE', ( #3215, #8238, #4903, #5652 ) ) ;
#17500 = EDGE_LOOP ( 'NONE', ( #7706, #2253 ) ) ;
#17501 = PLANE ( 'NONE',  #6619 ) ;
#17502 = TOROIDAL_SURFACE ( 'NONE', #15051, 15.88900348692940945, 3.000000000000000000 ) ;
#17503 = DIRECTION ( 'NONE',  ( -0.9876526153536336894, -0.1566598588826349503, 0.000000000000000000 ) ) ;
#17504 = ORIENTED_EDGE ( 'NONE', *, *, #14350, .T. ) ;
#17505 = EDGE_CURVE ( 'NONE', #4978, #1802, #6653, .T. ) ;
#17506 = ORIENTED_EDGE ( 'NONE', *, *, #9515, .F. ) ;
#17507 = FACE_OUTER_BOUND ( 'NONE', #14528, .T. ) ;
#17508 = CIRCLE ( 'NONE', #9303, 1.500000000000000888 ) ;
#17509 = FACE_BOUND ( 'NONE', #1382, .T. ) ;
#17510 = ADVANCED_FACE ( 'NONE', ( #17086 ), #4059, .F. ) ;
#17511 = EDGE_CURVE ( 'NONE', #4072, #3070, #14803, .T. ) ;
#17512 = EDGE_CURVE ( 'NONE', #8740, #2537, #11458, .T. ) ;
#17513 = FACE_OUTER_BOUND ( 'NONE', #6706, .T. ) ;
#17514 = DIRECTION ( 'NONE',  ( 0.000000000000000000, 0.000000000000000000, 1.000000000000000000 ) ) ;
#17515 = DIRECTION ( 'NONE',  ( -0.1566598588826321192, 0.9876526153536342445, 7.798540720466731404E-17 ) ) ;
#17516 = AXIS2_PLACEMENT_3D ( 'NONE', #9000, #4731, #13533 ) ;
#17517 = EDGE_CURVE ( 'NONE', #18393, #4379, #4443, .T. ) ;
#17518 = LINE ( 'NONE', #10285, #8160 ) ;
#17519 = ADVANCED_FACE ( 'NONE', ( #10600 ), #16120, .F. ) ;
#17520 = DIRECTION ( 'NONE',  ( -0.9723968097209878536, 0.2333333333333339199, 2.660152884942556746E-16 ) ) ;
#17521 = VERTEX_POINT ( 'NONE', #13350 ) ;
#17522 = FACE_OUTER_BOUND ( 'NONE', #7792, .T. ) ;
#17523 = CARTESIAN_POINT ( 'NONE',  ( -65.37641414873196766, 43.03264333350143289, -19.99999999999998934 ) ) ;
#17524 = ORIENTED_EDGE ( 'NONE', *, *, #2088, .T. ) ;
#17525 = LINE ( 'NONE', #11607, #2748 ) ;
#17526 = CIRCLE ( 'NONE', #15984, 1.500000000000000888 ) ;
#17527 = VECTOR ( 'NONE', #7807, 1000.000000000000000 ) ;
#17529 = ORIENTED_EDGE ( 'NONE', *, *, #3310, .T. ) ;
#17528 = DIRECTION ( 'NONE',  ( -0.1566598588826321747, 0.9876526153536343555, 0.000000000000000000 ) ) ;
#17530 = AXIS2_PLACEMENT_3D ( 'NONE', #2262, #10613, #10972 ) ;
#17531 = CIRCLE ( 'NONE', #14177, 1.500000000000000888 ) ;
#17532 = DIRECTION ( 'NONE',  ( -0.1566598588826321192, 0.9876526153536342445, 7.798540720466730171E-17 ) ) ;
#17533 = DIRECTION ( 'NONE',  ( -0.9876526153536336894, -0.1566598588826349503, 0.000000000000000000 ) ) ;
#17534 = EDGE_LOOP ( 'NONE', ( #15502, #5539 ) ) ;
#17535 = MECHANICAL_DESIGN_GEOMETRIC_PRESENTATION_REPRESENTATION (  '', ( #2067 ), #14179 ) ;
#17536 = CYLINDRICAL_SURFACE ( 'NONE', #13810, 150.0000000000000000 ) ;
#17537 = EDGE_CURVE ( 'NONE', #18596, #8348, #214, .T. ) ;
#17538 = DIRECTION ( 'NONE',  ( 3.208277787129350839E-17, 0.000000000000000000, -1.000000000000000000 ) ) ;
#17539 = CARTESIAN_POINT ( 'NONE',  ( -2.590506774712417748, -20.66068774275724707, 12.99038105676661026 ) ) ;
#17540 = AXIS2_PLACEMENT_3D ( 'NONE', #2673, #8466, #7067 ) ;
#17541 = CARTESIAN_POINT ( 'NONE',  ( -14.40270314877813895, -80.23978748569695085, 8.660254037844412167 ) ) ;
#17542 = DIRECTION ( 'NONE',  ( -0.9876526153536336894, -0.1566598588826350336, 0.000000000000000000 ) ) ;
#17543 = FACE_OUTER_BOUND ( 'NONE', #493, .T. ) ;
#17544 = ORIENTED_EDGE ( 'NONE', *, *, #1958, .T. ) ;
#17545 = AXIS2_PLACEMENT_3D ( 'NONE', #14491, #4527, #10210 ) ;
#17546 = EDGE_CURVE ( 'NONE', #16662, #18049, #468, .T. ) ;
#17547 = LINE ( 'NONE', #5794, #7833 ) ;
#17548 = AXIS2_PLACEMENT_3D ( 'NONE', #16729, #15560, #8363 ) ;
#17549 = CYLINDRICAL_SURFACE ( 'NONE', #16853, 1.500000000000001554 ) ;
#17550 = EDGE_CURVE ( 'NONE', #15127, #12774, #1150, .T. ) ;
#17551 = ADVANCED_FACE ( 'NONE', ( #11813 ), #8983, .F. ) ;
#17552 = CARTESIAN_POINT ( 'NONE',  ( -89.99999999999998579, -35.00000000000001421, 35.00000000000000000 ) ) ;
#17553 = LINE ( 'NONE', #13148, #14807 ) ;
#17554 = DIRECTION ( 'NONE',  ( -0.1566598588826321747, 0.9876526153536343555, 0.000000000000000000 ) ) ;
#17555 = ORIENTED_EDGE ( 'NONE', *, *, #16890, .T. ) ;
#17556 = VECTOR ( 'NONE', #5616, 1000.000000000000000 ) ;
#17557 = ORIENTED_EDGE ( 'NONE', *, *, #12754, .F. ) ;
#17558 = DIRECTION ( 'NONE',  ( 0.000000000000000000, -1.000000000000000000, 0.000000000000000000 ) ) ;
#17559 = VECTOR ( 'NONE', #14409, 1000.000000000000000 ) ;
#17560 = ORIENTED_EDGE ( 'NONE', *, *, #15257, .T. ) ;
#17561 = ORIENTED_EDGE ( 'NONE', *, *, #5520, .F. ) ;
#17562 = CARTESIAN_POINT ( 'NONE',  ( -24.81269062016911064, -24.18553456761645393, 17.32050807568881723 ) ) ;
#17563 = AXIS2_PLACEMENT_3D ( 'NONE', #16455, #13309, #7727 ) ;
#17564 = CARTESIAN_POINT ( 'NONE',  ( -12.92122422574768592, -80.00479769737299307, 8.660254037844412167 ) ) ;
#17565 = ORIENTED_EDGE ( 'NONE', *, *, #15504, .T. ) ;
#17566 = LINE ( 'NONE', #15636, #17358 ) ;
#17567 = AXIS2_PLACEMENT_3D ( 'NONE', #8850, #11744, #14710 ) ;
#17568 = AXIS2_PLACEMENT_3D ( 'NONE', #15917, #5410, #14222 ) ;
#17569 = VERTEX_POINT ( 'NONE', #17741 ) ;
#17570 = EDGE_CURVE ( 'NONE', #12897, #11672, #4440, .T. ) ;
#17571 = CIRCLE ( 'NONE', #16048, 1.500000000000001332 ) ;
#17572 = CARTESIAN_POINT ( 'NONE',  ( -60.16383145195930382, -24.73036655174043474, 8.660254037844417496 ) ) ;
#17573 = ORIENTED_EDGE ( 'NONE', *, *, #5589, .T. ) ;
#17574 = LINE ( 'NONE', #196, #16814 ) ;
#17575 = CIRCLE ( 'NONE', #3600, 1.500000000000001332 ) ;
#17576 = DIRECTION ( 'NONE',  ( -0.1566598588826321747, 0.9876526153536343555, 0.000000000000000000 ) ) ;
#17577 = CYLINDRICAL_SURFACE ( 'NONE', #16327, 1.500000000000001554 ) ;
#17578 = EDGE_CURVE ( 'NONE', #15920, #4102, #14438, .T. ) ;
#17579 = ORIENTED_EDGE ( 'NONE', *, *, #3353, .F. ) ;
#17580 = VERTEX_POINT ( 'NONE', #7319 ) ;
#17581 = AXIS2_PLACEMENT_3D ( 'NONE', #15722, #16276, #14401 ) ;
#17582 = ORIENTED_EDGE ( 'NONE', *, *, #10008, .F. ) ;
#17583 = DIRECTION ( 'NONE',  ( 0.000000000000000000, 0.000000000000000000, 1.000000000000000000 ) ) ;
#17584 = ORIENTED_EDGE ( 'NONE', *, *, #3201, .T. ) ;
#17585 = VECTOR ( 'NONE', #12519, 1000.000000000000000 ) ;
#17586 = FACE_BOUND ( 'NONE', #4844, .T. ) ;
#17587 = CARTESIAN_POINT ( 'NONE',  ( -312.1404785418517918, -2.850701963179328668, 9.951701414186818625E-16 ) ) ;
#17588 = CIRCLE ( 'NONE', #2738, 1.500000000000000000 ) ;
#17589 = ORIENTED_EDGE ( 'NONE', *, *, #17684, .F. ) ;
#17590 = CARTESIAN_POINT ( 'NONE',  ( -12.92122422574768592, -80.00479769737297886, -17.32050807568878525 ) ) ;
#17591 = CIRCLE ( 'NONE', #2122, 145.0000000000000284 ) ;
#17592 = VERTEX_POINT ( 'NONE', #3190 ) ;
#17593 = VERTEX_POINT ( 'NONE', #5883 ) ;
#17594 = CARTESIAN_POINT ( 'NONE',  ( -37.61253960958843834, -83.92129416943878084, -8.660254037844385522 ) ) ;
#17595 = AXIS2_PLACEMENT_3D ( 'NONE', #9812, #2603, #8105 ) ;
#17596 = CARTESIAN_POINT ( 'NONE',  ( -43.86756329862440396, -22.14547888017700927, 1.908195823574487804E-14 ) ) ;
#17598 = DIRECTION ( 'NONE',  ( -0.1566598588826321747, 0.9876526153536343555, 0.000000000000000000 ) ) ;
#17597 = CIRCLE ( 'NONE', #10298, 1.500000000000000444 ) ;
#17599 = DIRECTION ( 'NONE',  ( 1.000000000000000000, 0.000000000000000000, 0.000000000000000000 ) ) ;
#17600 = LINE ( 'NONE', #15870, #13761 ) ;
#17601 = CIRCLE ( 'NONE', #7007, 1.500000000000000888 ) ;
#17602 = CARTESIAN_POINT ( 'NONE',  ( -36.66452200441264608, -26.06545287420802737, -8.660254037844380193 ) ) ;
#17603 = ORIENTED_EDGE ( 'NONE', *, *, #13859, .F. ) ;
#17604 = VERTEX_POINT ( 'NONE', #6169 ) ;
#17605 = DIRECTION ( 'NONE',  ( -0.9876526153536341335, -0.1566598588826327021, 0.000000000000000000 ) ) ;
#17606 = ORIENTED_EDGE ( 'NONE', *, *, #12486, .F. ) ;
#17607 = EDGE_CURVE ( 'NONE', #4488, #11609, #3522, .T. ) ;
#17608 = AXIS2_PLACEMENT_3D ( 'NONE', #11999, #6267, #14874 ) ;
#17609 = CIRCLE ( 'NONE', #13327, 1.500000000000000000 ) ;
#17610 = LINE ( 'NONE', #7269, #13223 ) ;
#17611 = CARTESIAN_POINT ( 'NONE',  ( -28.22983976372896109, -82.43302551005379541, -12.99038105676658539 ) ) ;
#17612 = AXIS2_PLACEMENT_3D ( 'NONE', #8598, #16166, #11673 ) ;
#17613 = ORIENTED_EDGE ( 'NONE', *, *, #14426, .F. ) ;
#17614 = DIRECTION ( 'NONE',  ( 1.000000000000000000, 0.000000000000000000, 0.000000000000000000 ) ) ;
#17615 = EDGE_CURVE ( 'NONE', #14073, #18000, #14597, .T. ) ;
#17616 = VECTOR ( 'NONE', #13119, 1000.000000000000000 ) ;
#17617 = LINE ( 'NONE', #4592, #16958 ) ;
#17618 = AXIS2_PLACEMENT_3D ( 'NONE', #3168, #538, #13319 ) ;
#17619 = CARTESIAN_POINT ( 'NONE',  ( -44.56574292724172182, -27.31873174526908699, -17.32050807568878170 ) ) ;
#17620 = DIRECTION ( 'NONE',  ( -0.1566598588826321747, 0.9876526153536343555, 0.000000000000000000 ) ) ;
#17621 = PRESENTATION_STYLE_ASSIGNMENT (( #11411 ) ) ;
#17622 = CIRCLE ( 'NONE', #5508, 1.500000000000000444 ) ;
#17623 = ORIENTED_EDGE ( 'NONE', *, *, #8231, .F. ) ;
#17624 = CYLINDRICAL_SURFACE ( 'NONE', #6033, 1.500000000000001554 ) ;
#17625 = DIRECTION ( 'NONE',  ( 0.000000000000000000, 0.000000000000000000, 1.000000000000000000 ) ) ;
#17626 = AXIS2_PLACEMENT_3D ( 'NONE', #8141, #5210, #15053 ) ;
#17627 = CIRCLE ( 'NONE', #13353, 1.499999999999999556 ) ;
#17628 = DIRECTION ( 'NONE',  ( 0.000000000000000000, 0.000000000000000000, 1.000000000000000000 ) ) ;
#17629 = FACE_OUTER_BOUND ( 'NONE', #6287, .T. ) ;
#17630 = ORIENTED_EDGE ( 'NONE', *, *, #7378, .T. ) ;
#17631 = EDGE_LOOP ( 'NONE', ( #2070, #4309, #3752, #6035 ) ) ;
#17632 = CARTESIAN_POINT ( 'NONE',  ( -22.34355908178503469, -23.79388492040988012, 4.330127018922217630 ) ) ;
#17633 = ORIENTED_EDGE ( 'NONE', *, *, #12391, .F. ) ;
#17634 = ORIENTED_EDGE ( 'NONE', *, *, #353, .T. ) ;
#17635 = EDGE_CURVE ( 'NONE', #12573, #2063, #1148, .T. ) ;
#17636 = AXIS2_PLACEMENT_3D ( 'NONE', #9197, #14875, #478 ) ;
#17637 = EDGE_CURVE ( 'NONE', #9762, #16064, #8988, .T. ) ;
#17638 = EDGE_LOOP ( 'NONE', ( #15681, #1010, #14991, #11784 ) ) ;
#17639 = ORIENTED_EDGE ( 'NONE', *, *, #1970, .T. ) ;
#17640 = EDGE_CURVE ( 'NONE', #12774, #13253, #5963, .T. ) ;
#17641 = AXIS2_PLACEMENT_3D ( 'NONE', #12690, #18728, #14511 ) ;
#17642 = DIRECTION ( 'NONE',  ( -0.1566598588826321192, 0.9876526153536342445, 7.798540720466730171E-17 ) ) ;
#17643 = CARTESIAN_POINT ( 'NONE',  ( -72.71384246482016067, -31.78353772342409300, 17.32050807568881723 ) ) ;
#17644 = AXIS2_PLACEMENT_3D ( 'NONE', #4198, #7162, #15778 ) ;
#17645 = DIRECTION ( 'NONE',  ( -0.9876526153536341335, -0.1566598588826327021, 0.000000000000000000 ) ) ;
#17646 = CARTESIAN_POINT ( 'NONE',  ( -44.03228160938704860, -84.93958325217589334, -8.660254037844385522 ) ) ;
#17647 = CARTESIAN_POINT ( 'NONE',  ( -35.47251606811855851, -20.81387007967464697, 17.32050807568881723 ) ) ;
#17648 =( NAMED_UNIT ( * ) SI_UNIT ( $, .STERADIAN. ) SOLID_ANGLE_UNIT ( ) );
#17649 = AXIS2_PLACEMENT_3D ( 'NONE', #1517, #5873, #7305 ) ;
#17650 = PLANE ( 'NONE',  #12976 ) ;
#17651 = CARTESIAN_POINT ( 'NONE',  ( 2.881217619910392269, -77.49823995525089515, 4.330127018922209636 ) ) ;
#17652 = AXIS2_PLACEMENT_3D ( 'NONE', #2171, #12285, #11155 ) ;
#17653 = LINE ( 'NONE', #17552, #5355 ) ;
#17654 = CARTESIAN_POINT ( 'NONE',  ( -30.73860631229088369, -25.12549372091224598, -21.65063509461098334 ) ) ;
#17655 = ORIENTED_EDGE ( 'NONE', *, *, #2037, .F. ) ;
#17656 = EDGE_CURVE ( 'NONE', #9105, #3975, #2924, .T. ) ;
#17658 = ORIENTED_EDGE ( 'NONE', *, *, #1166, .F. ) ;
#17657 = DIRECTION ( 'NONE',  ( -0.1566598588826321192, 0.9876526153536342445, 7.798540720466730171E-17 ) ) ;
#17659 = AXIS2_PLACEMENT_3D ( 'NONE', #9003, #6183, #11914 ) ;
#17661 = ORIENTED_EDGE ( 'NONE', *, *, #5061, .T. ) ;
#17660 = EDGE_CURVE ( 'NONE', #13224, #8567, #2636, .T. ) ;
#17662 = DIRECTION ( 'NONE',  ( -0.1566598588826321192, 0.9876526153536342445, 7.798540720466730171E-17 ) ) ;
#17663 = ORIENTED_EDGE ( 'NONE', *, *, #17831, .F. ) ;
#17664 = ORIENTED_EDGE ( 'NONE', *, *, #7408, .T. ) ;
#17665 = LINE ( 'NONE', #4719, #14127 ) ;
#17666 = PRESENTATION_LAYER_ASSIGNMENT (  '', '', ( #388 ) ) ;
#17667 = EDGE_LOOP ( 'NONE', ( #3567, #4244, #18640, #4120 ) ) ;
#17668 = CARTESIAN_POINT ( 'NONE',  ( 59.44021041145192186, -44.12097743988036314, -130.3485206753969976 ) ) ;
#17669 = B_SPLINE_CURVE_WITH_KNOTS ( 'NONE', 3,
 ( #7997, #18074, #10815, #13673, #13758, #16530, #15104, #7913, #718, #6498, #12236, #5916, #17496, #4486, #10264, #3066, #14637, #13191 ),
 .UNSPECIFIED., .F., .F.,
 ( 4, 2, 2, 2, 2, 2, 2, 2, 4 ),
 ( 0.000000000000000000, 0.0006036110467293986622, 0.001207222093458797324, 0.001810833140188195661, 0.002414444186917594649, 0.003018055233646993202, 0.003621666280376390455, 0.004225277327105788142, 0.004828888373835185828 ),
 .UNSPECIFIED. ) ;
#17670 = FACE_OUTER_BOUND ( 'NONE', #6722, .T. ) ;
#17671 = CYLINDRICAL_SURFACE ( 'NONE', #15129, 1.500000000000001554 ) ;
#17672 = DIRECTION ( 'NONE',  ( -0.9876526153536336894, -0.1566598588826349503, 0.000000000000000000 ) ) ;
#17673 = CARTESIAN_POINT ( 'NONE',  ( 4.362696542940843081, -77.26325016692693737, -12.99038105676658539 ) ) ;
#17674 = VERTEX_POINT ( 'NONE', #15235 ) ;
#17675 = ORIENTED_EDGE ( 'NONE', *, *, #1576, .T. ) ;
#17676 = AXIS2_PLACEMENT_3D ( 'NONE', #10328, #10508, #6265 ) ;
#17677 = CARTESIAN_POINT ( 'NONE',  ( -4.526176995241833367, -78.67318889687062722, -8.660254037844385522 ) ) ;
#17678 = DIRECTION ( 'NONE',  ( -0.9876526153536341335, -0.1566598588826327021, 0.000000000000000000 ) ) ;
#17679 = ORIENTED_EDGE ( 'NONE', *, *, #683, .F. ) ;
#17680 = ORIENTED_EDGE ( 'NONE', *, *, #11636, .T. ) ;
#17681 = ORIENTED_EDGE ( 'NONE', *, *, #1446, .T. ) ;
#17682 = DIRECTION ( 'NONE',  ( 0.000000000000000000, 0.000000000000000000, 1.000000000000000000 ) ) ;
#17683 = FACE_BOUND ( 'NONE', #4414, .T. ) ;
#17684 = EDGE_CURVE ( 'NONE', #15676, #6194, #6895, .T. ) ;
#17685 = CARTESIAN_POINT ( 'NONE',  ( -3.000000000000000000, 4.898587196589412829E-16, 32.00000000000000000 ) ) ;
#17686 = EDGE_CURVE ( 'NONE', #13070, #1457, #18734, .T. ) ;
#17687 = ORIENTED_EDGE ( 'NONE', *, *, #4241, .T. ) ;
#17688 = CIRCLE ( 'NONE', #14927, 1.500000000000000000 ) ;
#17689 = CARTESIAN_POINT ( 'NONE',  ( -73.49714175923330117, -26.84527464665595176, -17.32050807568878170 ) ) ;
#17690 = ORIENTED_EDGE ( 'NONE', *, *, #1850, .T. ) ;
#17691 = ADVANCED_FACE ( 'NONE', ( #2250 ), #10961, .F. ) ;
#17692 = ORIENTED_EDGE ( 'NONE', *, *, #1647, .F. ) ;
#17693 = ORIENTED_EDGE ( 'NONE', *, *, #3902, .T. ) ;
#17694 = CARTESIAN_POINT ( 'NONE',  ( -66.78792677269838407, -30.84357857012830095, 12.99038105676661736 ) ) ;
#17695 = DIRECTION ( 'NONE',  ( -0.9876526153536336894, -0.1566598588826350336, 0.000000000000000000 ) ) ;
#17696 = DIRECTION ( 'NONE',  ( -0.1566598588826321747, 0.9876526153536343555, 0.000000000000000000 ) ) ;
#17697 = CARTESIAN_POINT ( 'NONE',  ( -74.62210677719829732, 46.96672731380024146, -2.500000000000000000 ) ) ;
#17698 = CARTESIAN_POINT ( 'NONE',  ( -25.80034323552273534, -24.34219442649909126, 12.99038105676661736 ) ) ;
#17699 = VERTEX_POINT ( 'NONE', #18118 ) ;
#17700 = ORIENTED_EDGE ( 'NONE', *, *, #3881, .F. ) ;
#17701 = AXIS2_PLACEMENT_3D ( 'NONE', #9373, #18238, #11157 ) ;
#17702 = CARTESIAN_POINT ( 'NONE',  ( -62.00000000000000000, 0.000000000000000000, 25.00000000000000000 ) ) ;
#17703 = DIRECTION ( 'NONE',  ( 0.000000000000000000, 0.000000000000000000, 1.000000000000000000 ) ) ;
#17704 = DIRECTION ( 'NONE',  ( -0.9876526153536336894, -0.1566598588826350336, 0.000000000000000000 ) ) ;
#17705 = VERTEX_POINT ( 'NONE', #3843 ) ;
#17706 = LINE ( 'NONE', #7536, #52 ) ;
#17707 = EDGE_CURVE ( 'NONE', #3093, #1326, #13907, .T. ) ;
#17708 = CARTESIAN_POINT ( 'NONE',  ( -76.90911978745816668, -45.00000000000000711, 20.00000000000002132 ) ) ;
#17709 = EDGE_CURVE ( 'NONE', #1903, #14341, #16567, .T. ) ;
#17710 = DIRECTION ( 'NONE',  ( 1.000000000000000000, 0.000000000000000000, 0.000000000000000000 ) ) ;
#17711 = DIRECTION ( 'NONE',  ( 0.9868632313631133801, -0.1615579233078772714, 0.000000000000000000 ) ) ;
#17712 = VERTEX_POINT ( 'NONE', #7757 ) ;
#17713 = DIRECTION ( 'NONE',  ( -0.9876526153536341335, -0.1566598588826327021, 0.000000000000000000 ) ) ;
#17714 = FACE_OUTER_BOUND ( 'NONE', #9974, .T. ) ;
#17715 = EDGE_CURVE ( 'NONE', #15200, #13047, #8084, .T. ) ;
#17716 = CYLINDRICAL_SURFACE ( 'NONE', #16198, 1.500000000000001554 ) ;
#17717 = ORIENTED_EDGE ( 'NONE', *, *, #7059, .F. ) ;
#17718 = ORIENTED_EDGE ( 'NONE', *, *, #12663, .F. ) ;
#17719 = CYLINDRICAL_SURFACE ( 'NONE', #2450, 1.500000000000000666 ) ;
#17720 = ORIENTED_EDGE ( 'NONE', *, *, #17746, .F. ) ;
#17721 = ORIENTED_EDGE ( 'NONE', *, *, #14075, .T. ) ;
#17722 = CIRCLE ( 'NONE', #16185, 1.500000000000000888 ) ;
#17723 = DIRECTION ( 'NONE',  ( 0.9539392014169441047, 0.3000000000000046518, 0.000000000000000000 ) ) ;
#17724 = EDGE_CURVE ( 'NONE', #14381, #7806, #18107, .T. ) ;
#17725 = CARTESIAN_POINT ( 'NONE',  ( -38.92930022185626626, -21.36217958576384390, -17.32050807568878170 ) ) ;
#17726 = ORIENTED_EDGE ( 'NONE', *, *, #13156, .F. ) ;
#17727 = DIRECTION ( 'NONE',  ( -0.000000000000000000, -0.000000000000000000, -1.000000000000000000 ) ) ;
#17728 = CARTESIAN_POINT ( 'NONE',  ( -40.61513246582718750, -26.69209230973856251, -21.65063509461098334 ) ) ;
#17729 = EDGE_LOOP ( 'NONE', ( #9578, #383 ) ) ;
#17730 = DIRECTION ( 'NONE',  ( -0.9876526153536341335, -0.1566598588826327021, 0.000000000000000000 ) ) ;
#17731 = EDGE_CURVE ( 'NONE', #6405, #6362, #5367, .T. ) ;
#17732 = DIRECTION ( 'NONE',  ( -0.1566598588826321192, 0.9876526153536342445, 7.798540720466730171E-17 ) ) ;
#17733 = LINE ( 'NONE', #11982, #486 ) ;
#17734 = CIRCLE ( 'NONE', #10137, 1.500000000000000000 ) ;
#17735 = ADVANCED_FACE ( 'NONE', ( #563 ), #16685, .F. ) ;
#17736 = DIRECTION ( 'NONE',  ( 0.000000000000000000, 0.000000000000000000, 1.000000000000000000 ) ) ;
#17738 = ORIENTED_EDGE ( 'NONE', *, *, #16789, .T. ) ;
#17737 = CARTESIAN_POINT ( 'NONE',  ( -11.93357161039406300, -79.84813783849035929, -12.99038105676658539 ) ) ;
#17739 = ORIENTED_EDGE ( 'NONE', *, *, #13175, .F. ) ;
#17740 = EDGE_LOOP ( 'NONE', ( #16620, #2234, #5713, #710 ) ) ;
#17741 = CARTESIAN_POINT ( 'NONE',  ( -10.28737437660098131, -16.81904367816753165, -12.99038105676658006 ) ) ;
#17742 = VERTEX_POINT ( 'NONE', #12279 ) ;
#17743 = EDGE_LOOP ( 'NONE', ( #12191, #12801 ) ) ;
#17744 = DIRECTION ( 'NONE',  ( 0.000000000000000000, 0.000000000000000000, 1.000000000000000000 ) ) ;
#17745 = FACE_OUTER_BOUND ( 'NONE', #14788, .T. ) ;
#17746 = EDGE_CURVE ( 'NONE', #11470, #17593, #9899, .T. ) ;
#17747 = DIRECTION ( 'NONE',  ( -0.9876526153536341335, -0.1566598588826327021, 0.000000000000000000 ) ) ;
#17748 = CIRCLE ( 'NONE', #781, 1.500000000000000888 ) ;
#17749 = VERTEX_POINT ( 'NONE', #15150 ) ;
#17750 = PLANE ( 'NONE',  #8838 ) ;
#17751 = ADVANCED_FACE ( 'NONE', ( #6358 ), #9555, .F. ) ;
#17752 = EDGE_CURVE ( 'NONE', #1312, #12413, #14955, .T. ) ;
#17753 = DIRECTION ( 'NONE',  ( 0.1856185419698759831, -0.9826218788918641422, 0.000000000000000000 ) ) ;
#17754 = EDGE_CURVE ( 'NONE', #5889, #4539, #12092, .T. ) ;
#17755 = DIRECTION ( 'NONE',  ( -0.1566598588826321747, 0.9876526153536343555, 0.000000000000000000 ) ) ;
#17756 = PLANE ( 'NONE',  #5068 ) ;
#17757 = ORIENTED_EDGE ( 'NONE', *, *, #12239, .T. ) ;
#17758 = FACE_BOUND ( 'NONE', #16582, .T. ) ;
#17759 = ADVANCED_FACE ( 'NONE', ( #2342 ), #17939, .F. ) ;
#17760 = CARTESIAN_POINT ( 'NONE',  ( -309.1404785418517918, -2.850701963179326892, -15.88900348692940945 ) ) ;
#17761 = ORIENTED_EDGE ( 'NONE', *, *, #6987, .T. ) ;
#17762 = DIRECTION ( 'NONE',  ( -0.1566598588826321747, 0.9876526153536343555, 0.000000000000000000 ) ) ;
#17763 = DIRECTION ( 'NONE',  ( -0.1566598588826321747, 0.9876526153536343555, 0.000000000000000000 ) ) ;
#17764 = VECTOR ( 'NONE', #15140, 1000.000000000000114 ) ;
#17765 = ORIENTED_EDGE ( 'NONE', *, *, #4609, .F. ) ;
#17766 = ORIENTED_EDGE ( 'NONE', *, *, #220, .F. ) ;
#17767 = ORIENTED_EDGE ( 'NONE', *, *, #13285, .F. ) ;
#17768 = DIRECTION ( 'NONE',  ( -0.1566598588826321192, 0.9876526153536342445, 7.798540720466730171E-17 ) ) ;
#17769 = ORIENTED_EDGE ( 'NONE', *, *, #17709, .F. ) ;
#17770 = ORIENTED_EDGE ( 'NONE', *, *, #10438, .F. ) ;
#17771 = FACE_BOUND ( 'NONE', #4268, .T. ) ;
#17772 = VERTEX_POINT ( 'NONE', #851 ) ;
#17773 = DIRECTION ( 'NONE',  ( -0.9876526153536341335, -0.1566598588826327021, 0.000000000000000000 ) ) ;
#17774 = ORIENTED_EDGE ( 'NONE', *, *, #5615, .T. ) ;
#17775 = EDGE_CURVE ( 'NONE', #16602, #2144, #18431, .T. ) ;
#17776 = EDGE_LOOP ( 'NONE', ( #12209, #13663 ) ) ;
#17777 = DIRECTION ( 'NONE',  ( -0.9876526153536344665, -0.1566598588826304539, 0.000000000000000000 ) ) ;
#17778 = FACE_BOUND ( 'NONE', #15955, .T. ) ;
#17779 = CYLINDRICAL_SURFACE ( 'NONE', #1590, 1.500000000000000888 ) ;
#17780 = PLANE ( 'NONE',  #6377 ) ;
#17781 = DIRECTION ( 'NONE',  ( -0.1566598588826321747, 0.9876526153536343555, 0.000000000000000000 ) ) ;
#17782 = EDGE_CURVE ( 'NONE', #8619, #14167, #17192, .T. ) ;
#17783 = DIRECTION ( 'NONE',  ( 1.000000000000000000, 0.000000000000000000, -0.000000000000000000 ) ) ;
#17784 = DIRECTION ( 'NONE',  ( 0.8007491221077702725, -0.5989998693185459855, 0.000000000000000000 ) ) ;
#17785 = ORIENTED_EDGE ( 'NONE', *, *, #8676, .T. ) ;
#17786 = ORIENTED_EDGE ( 'NONE', *, *, #14106, .F. ) ;
#17787 = DIRECTION ( 'NONE',  ( -0.1566598588826321192, 0.9876526153536342445, 7.798540720466730171E-17 ) ) ;
#17788 = CIRCLE ( 'NONE', #14432, 12.74754878398196567 ) ;
#17789 = DIRECTION ( 'NONE',  ( 0.000000000000000000, 0.000000000000000000, 1.000000000000000000 ) ) ;
#17790 = CIRCLE ( 'NONE', #14738, 1.500000000000000888 ) ;
#17791 = EDGE_LOOP ( 'NONE', ( #10604, #2657 ) ) ;
#17792 = CARTESIAN_POINT ( 'NONE',  ( 6.831828081324923474, -76.87160051972034580, -17.32050807568878525 ) ) ;
#17793 = AXIS2_PLACEMENT_3D ( 'NONE', #6733, #9364, #13516 ) ;
#17794 = FACE_BOUND ( 'NONE', #10456, .T. ) ;
#17795 = VECTOR ( 'NONE', #16471, 1000.000000000000000 ) ;
#17796 = VECTOR ( 'NONE', #2820, 1000.000000000000000 ) ;
#17797 = LINE ( 'NONE', #4774, #2763 ) ;
#17798 = DIRECTION ( 'NONE',  ( 0.000000000000000000, 0.000000000000000000, 1.000000000000000000 ) ) ;
#17799 = CYLINDRICAL_SURFACE ( 'NONE', #12372, 1.500000000000001554 ) ;
#17800 = DIRECTION ( 'NONE',  ( -0.1566598588826321192, 0.9876526153536342445, 7.798540720466730171E-17 ) ) ;
#17801 = AXIS2_PLACEMENT_3D ( 'NONE', #15665, #4392, #50 ) ;
#17802 = DIRECTION ( 'NONE',  ( -0.1566598588826321192, 0.9876526153536342445, 7.798540720466731404E-17 ) ) ;
#17803 = EDGE_CURVE ( 'NONE', #11811, #7186, #9587, .T. ) ;
#17804 = AXIS2_PLACEMENT_3D ( 'NONE', #17330, #4313, #10089 ) ;
#17805 = PLANE ( 'NONE',  #11923 ) ;
#17806 = ORIENTED_EDGE ( 'NONE', *, *, #15829, .F. ) ;
#17807 = VERTEX_POINT ( 'NONE', #16070 ) ;
#17808 = CARTESIAN_POINT ( 'NONE',  ( -26.74836084069852404, -82.19803572172983763, -21.65063509461098690 ) ) ;
#17809 = EDGE_CURVE ( 'NONE', #4926, #3971, #5682, .T. ) ;
#17810 = EDGE_LOOP ( 'NONE', ( #6189, #1743, #7222, #14512 ) ) ;
#17811 = AXIS2_PLACEMENT_3D ( 'NONE', #8600, #1396, #7181 ) ;
#17812 = EDGE_CURVE ( 'NONE', #2898, #11338, #14008, .T. ) ;
#17813 = ORIENTED_EDGE ( 'NONE', *, *, #8908, .T. ) ;
#17814 = CARTESIAN_POINT ( 'NONE',  ( -48.02252708097940825, -27.86704125135829813, -8.660254037844380193 ) ) ;
#17815 = AXIS2_PLACEMENT_3D ( 'NONE', #6181, #769, #2084 ) ;
#17816 = VERTEX_POINT ( 'NONE', #14366 ) ;
#17817 = DIRECTION ( 'NONE',  ( -0.9876526153536341335, -0.1566598588826327021, 0.000000000000000000 ) ) ;
#17818 = DIRECTION ( 'NONE',  ( -0.1566598588826321192, 0.9876526153536342445, 7.798540720466731404E-17 ) ) ;
#17819 = EDGE_LOOP ( 'NONE', ( #1392, #4555 ) ) ;
#17820 = DIRECTION ( 'NONE',  ( -0.9826218788918642533, -0.1856185419698762884, 0.000000000000000000 ) ) ;
#17821 = AXIS2_PLACEMENT_3D ( 'NONE', #18020, #4977, #16571 ) ;
#17822 = CARTESIAN_POINT ( 'NONE',  ( -58.68235252892886678, -24.49537676341647696, -17.32050807568878170 ) ) ;
#17823 = CARTESIAN_POINT ( 'NONE',  ( -41.56315007100297265, -84.54793360496931598, -21.65063509461098690 ) ) ;
#17824 = FACE_BOUND ( 'NONE', #1292, .T. ) ;
#17825 = DIRECTION ( 'NONE',  ( -0.1566598588826321192, 0.9876526153536342445, 7.798540720466730171E-17 ) ) ;
#17826 = CARTESIAN_POINT ( 'NONE',  ( -67.24211807019732134, -88.62108993591773753, -17.32050807568878525 ) ) ;
#17828 = EDGE_LOOP ( 'NONE', ( #11454, #6890 ) ) ;
#17827 = DIRECTION ( 'NONE',  ( -0.1566598588826321192, 0.9876526153536342445, 7.798540720466730171E-17 ) ) ;
#17829 = AXIS2_PLACEMENT_3D ( 'NONE', #12577, #10969, #14017 ) ;
#17830 = DIRECTION ( 'NONE',  ( -0.1566598588826321192, 0.9876526153536342445, 7.798540720466731404E-17 ) ) ;
#17831 = EDGE_CURVE ( 'NONE', #8230, #9109, #1437, .T. ) ;
#17832 = ORIENTED_EDGE ( 'NONE', *, *, #1471, .T. ) ;
#17833 = ORIENTED_EDGE ( 'NONE', *, *, #13522, .T. ) ;
#17834 = DIRECTION ( 'NONE',  ( -0.1566598588826321192, 0.9876526153536342445, 7.798540720466730171E-17 ) ) ;
#17835 = AXIS2_PLACEMENT_3D ( 'NONE', #13111, #9897, #18764 ) ;
#17836 = DIRECTION ( 'NONE',  ( -0.9876526153536336894, -0.1566598588826350336, 0.000000000000000000 ) ) ;
#17837 = EDGE_CURVE ( 'NONE', #12413, #482, #11592, .T. ) ;
#17838 = CIRCLE ( 'NONE', #15082, 1.500000000000000888 ) ;
#17839 = ORIENTED_EDGE ( 'NONE', *, *, #13276, .F. ) ;
#17840 = DIRECTION ( 'NONE',  ( 0.9723968097209870765, 0.2333333333333372228, 0.000000000000000000 ) ) ;
#17841 = VECTOR ( 'NONE', #5242, 1000.000000000000000 ) ;
#17842 = CARTESIAN_POINT ( 'NONE',  ( -31.72625892764450484, -25.28215357979487266, -8.660254037844380193 ) ) ;
#17843 = CARTESIAN_POINT ( 'NONE',  ( -10.98555400521827963, -21.99229654325962002, -4.330127018922181215 ) ) ;
#17844 = DIRECTION ( 'NONE',  ( -0.000000000000000000, -0.000000000000000000, -1.000000000000000000 ) ) ;
#17845 = DIRECTION ( 'NONE',  ( -0.1566598588826321192, 0.9876526153536342445, 7.798540720466731404E-17 ) ) ;
#17846 = CARTESIAN_POINT ( 'NONE',  ( -62.79768130110601021, -87.91612057094592103, 12.99038105676661203 ) ) ;
#17847 = CARTESIAN_POINT ( 'NONE',  ( -306.0881213225399051, -2.850701963179328668, 15.83618137761393463 ) ) ;
#17848 = ORIENTED_EDGE ( 'NONE', *, *, #10351, .F. ) ;
#17849 = CIRCLE ( 'NONE', #3873, 1.500000000000000888 ) ;
#17850 = CARTESIAN_POINT ( 'NONE',  ( -5.842937607509656850, -16.11407431319567962, -17.32050807568878170 ) ) ;
#17851 = ORIENTED_EDGE ( 'NONE', *, *, #4273, .T. ) ;
#17852 = CARTESIAN_POINT ( 'NONE',  ( -34.97868976044173195, -20.73554015023333363, 12.99038105676661736 ) ) ;
#17853 = AXIS2_PLACEMENT_3D ( 'NONE', #5431, #9507, #15477 ) ;
#17854 = AXIS2_PLACEMENT_3D ( 'NONE', #971, #2467, #11161 ) ;
#17855 = CARTESIAN_POINT ( 'NONE',  ( -55.22556837519117323, -23.94706725732726937, -8.660254037844380193 ) ) ;
#17856 = VECTOR ( 'NONE', #15431, 1000.000000000000227 ) ;
#17857 = ORIENTED_EDGE ( 'NONE', *, *, #3269, .F. ) ;
#17858 = EDGE_LOOP ( 'NONE', ( #13555, #9558, #17201, #6996 ) ) ;
#17859 = ORIENTED_EDGE ( 'NONE', *, *, #3540, .F. ) ;
#17860 = CYLINDRICAL_SURFACE ( 'NONE', #6555, 1.500000000000001554 ) ;
#17861 = EDGE_CURVE ( 'NONE', #8059, #4101, #3817, .T. ) ;
#17862 = EDGE_CURVE ( 'NONE', #6801, #442, #8687, .T. ) ;
#17863 = ORIENTED_EDGE ( 'NONE', *, *, #3619, .T. ) ;
#17864 = FACE_BOUND ( 'NONE', #9062, .T. ) ;
#17865 = EDGE_CURVE ( 'NONE', #11250, #6623, #2453, .T. ) ;
#17866 = AXIS2_PLACEMENT_3D ( 'NONE', #5543, #14435, #11576 ) ;
#17867 = CARTESIAN_POINT ( 'NONE',  ( -13.41505053342451426, -80.08312762681431707, -21.65063509461098690 ) ) ;
#17868 = AXIS2_PLACEMENT_3D ( 'NONE', #2363, #3685, #15255 ) ;
#17869 = ORIENTED_EDGE ( 'NONE', *, *, #8296, .F. ) ;
#17870 = CIRCLE ( 'NONE', #9682, 1.500000000000000444 ) ;
#17871 = VECTOR ( 'NONE', #15691, 1000.000000000000000 ) ;
#17872 = AXIS2_PLACEMENT_3D ( 'NONE', #9524, #9892, #920 ) ;
#17873 = CIRCLE ( 'NONE', #9689, 1.500000000000000888 ) ;
#17874 = EDGE_LOOP ( 'NONE', ( #2445, #13543 ) ) ;
#17875 = CARTESIAN_POINT ( 'NONE',  ( -52.42732883989287274, -86.27119205267827340, 17.32050807568881368 ) ) ;
#17876 = SHAPE_REPRESENTATION ( 'Lower Hopper Receiver Handle Arm', ( #18772 ), #5087 ) ;
#17877 = CARTESIAN_POINT ( 'NONE',  ( 73.09088021254186174, 1.387778780781445676E-14, -7.500000000000000000 ) ) ;
#17878 = VERTEX_POINT ( 'NONE', #1391 ) ;
#17879 = DIRECTION ( 'NONE',  ( -0.9876526153536336894, -0.1566598588826349503, 0.000000000000000000 ) ) ;
#17880 = ORIENTED_EDGE ( 'NONE', *, *, #10577, .T. ) ;
#17881 = DIRECTION ( 'NONE',  ( 0.000000000000000000, 0.000000000000000000, 1.000000000000000000 ) ) ;
#17882 = DIRECTION ( 'NONE',  ( -0.1566598588826321747, 0.9876526153536343555, 0.000000000000000000 ) ) ;
#17883 = AXIS2_PLACEMENT_3D ( 'NONE', #5403, #2644, #18341 ) ;
#17884 = FACE_OUTER_BOUND ( 'NONE', #16815, .T. ) ;
#17885 = DIRECTION ( 'NONE',  ( -0.000000000000000000, -0.000000000000000000, -1.000000000000000000 ) ) ;
#17886 = ORIENTED_EDGE ( 'NONE', *, *, #8806, .F. ) ;
#17887 = ORIENTED_EDGE ( 'NONE', *, *, #3274, .T. ) ;
#17888 = DIRECTION ( 'NONE',  ( -0.000000000000000000, -0.000000000000000000, -1.000000000000000000 ) ) ;
#17889 = ADVANCED_FACE ( 'NONE', ( #8762 ), #1661, .F. ) ;
#17890 = DIRECTION ( 'NONE',  ( -1.000000000000000000, 0.000000000000000000, 0.000000000000000000 ) ) ;
#17891 = AXIS2_PLACEMENT_3D ( 'NONE', #13561, #8857, #13384 ) ;
#17892 = DIRECTION ( 'NONE',  ( -0.1566598588826321192, 0.9876526153536342445, 7.798540720466730171E-17 ) ) ;
#17893 = DIRECTION ( 'NONE',  ( 1.000000000000000000, 0.000000000000000000, 0.000000000000000000 ) ) ;
#17894 = CIRCLE ( 'NONE', #13005, 1.499999999999999556 ) ;
#17895 = ADVANCED_FACE ( 'NONE', ( #7440 ), #13114, .F. ) ;
#17896 = ORIENTED_EDGE ( 'NONE', *, *, #4609, .T. ) ;
#17897 = ORIENTED_EDGE ( 'NONE', *, *, #17550, .T. ) ;
#17898 = DIRECTION ( 'NONE',  ( 1.000000000000000000, 0.000000000000000000, 0.000000000000000000 ) ) ;
#17899 = ORIENTED_EDGE ( 'NONE', *, *, #7312, .F. ) ;
#17900 = CIRCLE ( 'NONE', #9709, 1.500000000000001332 ) ;
#17901 = DIRECTION ( 'NONE',  ( -1.000000000000000000, 0.000000000000000000, 0.000000000000000000 ) ) ;
#17902 = LINE ( 'NONE', #10656, #5118 ) ;
#17903 = LINE ( 'NONE', #6222, #16639 ) ;
#17904 = CIRCLE ( 'NONE', #13312, 1.500000000000000888 ) ;
#17905 = DIRECTION ( 'NONE',  ( -0.1566598588826321192, 0.9876526153536342445, 7.798540720466730171E-17 ) ) ;
#17906 = VECTOR ( 'NONE', #12258, 1000.000000000000000 ) ;
#17907 = FACE_OUTER_BOUND ( 'NONE', #12832, .T. ) ;
#17908 = LINE ( 'NONE', #17999, #12858 ) ;
#17909 = DIRECTION ( 'NONE',  ( 0.000000000000000000, 0.000000000000000000, 1.000000000000000000 ) ) ;
#17910 = ORIENTED_EDGE ( 'NONE', *, *, #7361, .T. ) ;
#17911 = ORIENTED_EDGE ( 'NONE', *, *, #3676, .T. ) ;
#17912 = CARTESIAN_POINT ( 'NONE',  ( -41.39843176024034221, -21.75382923297042481, -21.65063509461097979 ) ) ;
#17913 = ORIENTED_EDGE ( 'NONE', *, *, #9817, .F. ) ;
#17914 = EDGE_LOOP ( 'NONE', ( #5627, #2040, #11490, #13643 ) ) ;
#17915 = ORIENTED_EDGE ( 'NONE', *, *, #872, .F. ) ;
#17916 = AXIS2_PLACEMENT_3D ( 'NONE', #2615, #8682, #4112 ) ;
#17917 = AXIS2_PLACEMENT_3D ( 'NONE', #14842, #1863, #5060 ) ;
#17918 = EDGE_LOOP ( 'NONE', ( #4938, #5801, #1685, #6261 ) ) ;
#17919 = FACE_OUTER_BOUND ( 'NONE', #16160, .T. ) ;
#17920 = ADVANCED_FACE ( 'NONE', ( #12920 ), #6014, .F. ) ;
#17921 = AXIS2_PLACEMENT_3D ( 'NONE', #15509, #2428, #8215 ) ;
#17922 = EDGE_LOOP ( 'NONE', ( #17663, #5438 ) ) ;
#17923 = DIRECTION ( 'NONE',  ( -0.1566598588826321192, 0.9876526153536342445, 7.798540720466730171E-17 ) ) ;
#17924 = EDGE_CURVE ( 'NONE', #5396, #8469, #9302, .T. ) ;
#17925 = FACE_OUTER_BOUND ( 'NONE', #15361, .T. ) ;
#17926 = CYLINDRICAL_SURFACE ( 'NONE', #2187, 1.500000000000001554 ) ;
#17927 = CARTESIAN_POINT ( 'NONE',  ( -70.24471092643608472, -31.39188807621751209, -21.65063509461098334 ) ) ;
#17928 = AXIS2_PLACEMENT_3D ( 'NONE', #15996, #17076, #5787 ) ;
#17929 = EDGE_CURVE ( 'NONE', #8901, #6017, #6909, .T. ) ;
#17930 = DIRECTION ( 'NONE',  ( -0.1566598588826321192, 0.9876526153536342445, 7.798540720466731404E-17 ) ) ;
#17931 = CARTESIAN_POINT ( 'NONE',  ( -64.60826822105063627, -25.43533591671227967, 4.330127018922218518 ) ) ;
#17932 = DIRECTION ( 'NONE',  ( -0.1566598588826321192, 0.9876526153536342445, 7.798540720466731404E-17 ) ) ;
#17933 = EDGE_LOOP ( 'NONE', ( #13620, #10788, #1060, #2141 ) ) ;
#17934 = AXIS2_PLACEMENT_3D ( 'NONE', #3713, #16926, #6689 ) ;
#17935 = CARTESIAN_POINT ( 'NONE',  ( -90.00000000000000000, 34.99999999999999289, 35.00000000000000000 ) ) ;
#17936 = CARTESIAN_POINT ( 'NONE',  ( -4.526176995241833367, -78.67318889687062722, 17.32050807568880657 ) ) ;
#17938 = ORIENTED_EDGE ( 'NONE', *, *, #9265, .F. ) ;
#17937 = DIRECTION ( 'NONE',  ( -0.9876526153536336894, -0.1566598588826349503, 0.000000000000000000 ) ) ;
#17939 = CYLINDRICAL_SURFACE ( 'NONE', #3228, 1.500000000000000888 ) ;
#17940 = ORIENTED_EDGE ( 'NONE', *, *, #5040, .T. ) ;
#17941 = VERTEX_POINT ( 'NONE', #11764 ) ;
#17942 = AXIS2_PLACEMENT_3D ( 'NONE', #5506, #8150, #11346 ) ;
#17943 = DIRECTION ( 'NONE',  ( -0.1566598588826321747, 0.9876526153536343555, 0.000000000000000000 ) ) ;
#17944 = VERTEX_POINT ( 'NONE', #2808 ) ;
#17945 = AXIS2_PLACEMENT_3D ( 'NONE', #15342, #18243, #2354 ) ;
#17946 = CARTESIAN_POINT ( 'NONE',  ( -45.55339554259532520, -27.47539160415171722, 21.65063509461101887 ) ) ;
#17947 = DIRECTION ( 'NONE',  ( 0.000000000000000000, 0.000000000000000000, 1.000000000000000000 ) ) ;
#17948 = CARTESIAN_POINT ( 'NONE',  ( -128.7754985213481689, -14.93136237110436859, -4.052748550462855093 ) ) ;
#17949 = EDGE_CURVE ( 'NONE', #1506, #12466, #231, .T. ) ;
#17950 = FACE_OUTER_BOUND ( 'NONE', #13778, .T. ) ;
#17951 = CARTESIAN_POINT ( 'NONE',  ( -3.578159390066044665, -20.81734760163988440, 1.522258424776792809E-14 ) ) ;
#17952 = CARTESIAN_POINT ( 'NONE',  ( 5.481473465377021625, 12.88229205725314763, 25.00000000000000000 ) ) ;
#17953 = ORIENTED_EDGE ( 'NONE', *, *, #6239, .T. ) ;
#17954 = AXIS2_PLACEMENT_3D ( 'NONE', #16706, #2268, #6651 ) ;
#17955 = DIRECTION ( 'NONE',  ( 0.000000000000000000, 0.000000000000000000, 1.000000000000000000 ) ) ;
#17956 = ORIENTED_EDGE ( 'NONE', *, *, #807, .T. ) ;
#17957 = DIRECTION ( 'NONE',  ( -2.671473304378624222E-16, -0.000000000000000000, -1.000000000000000000 ) ) ;
#17958 = ADVANCED_FACE ( 'NONE', ( #9659 ), #17502, .T. ) ;
#17959 = LINE ( 'NONE', #774, #5436 ) ;
#17960 = VERTEX_POINT ( 'NONE', #4210 ) ;
#17961 = VERTEX_POINT ( 'NONE', #5750 ) ;
#17962 = ORIENTED_EDGE ( 'NONE', *, *, #4777, .T. ) ;
#17963 = CARTESIAN_POINT ( 'NONE',  ( -29.21749237908258223, -82.58968536893642920, 8.660254037844412167 ) ) ;
#17964 = FACE_BOUND ( 'NONE', #7815, .T. ) ;
#17965 = CARTESIAN_POINT ( 'NONE',  ( -79.13358446461874962, -32.80182680616118773, -17.32050807568878170 ) ) ;
#17966 = EDGE_LOOP ( 'NONE', ( #5910, #10022, #1286, #7045 ) ) ;
#17967 = VECTOR ( 'NONE', #9582, 1000.000000000000000 ) ;
#17968 = EDGE_CURVE ( 'NONE', #6198, #3838, #5054, .T. ) ;
#17969 = FACE_BOUND ( 'NONE', #3075, .T. ) ;
#17970 = ORIENTED_EDGE ( 'NONE', *, *, #9153, .T. ) ;
#17971 = ORIENTED_EDGE ( 'NONE', *, *, #14106, .T. ) ;
#17972 = LINE ( 'NONE', #12031, #15752 ) ;
#17973 = ORIENTED_EDGE ( 'NONE', *, *, #8979, .F. ) ;
#17974 = CARTESIAN_POINT ( 'NONE',  ( -57.20087360589841552, -24.26038697509253339, -17.32050807568878170 ) ) ;
#17975 = ADVANCED_FACE ( 'NONE', ( #15876 ), #2877, .F. ) ;
#17976 = FACE_OUTER_BOUND ( 'NONE', #3506, .T. ) ;
#17977 = CARTESIAN_POINT ( 'NONE',  ( -11.76885329963143434, -17.05403346649147878, -4.330127018922180326 ) ) ;
#17978 = EDGE_LOOP ( 'NONE', ( #3405, #16629, #17675, #16421 ) ) ;
#17979 = EDGE_LOOP ( 'NONE', ( #687, #17863, #15567, #11664 ) ) ;
#17980 = DIRECTION ( 'NONE',  ( 1.000000000000000000, 0.000000000000000000, 0.000000000000000000 ) ) ;
#17981 = LINE ( 'NONE', #10547, #843 ) ;
#17982 = CYLINDRICAL_SURFACE ( 'NONE', #14455, 1.500000000000001554 ) ;
#17983 = ORIENTED_EDGE ( 'NONE', *, *, #3998, .F. ) ;
#17984 = VECTOR ( 'NONE', #6077, 1000.000000000000000 ) ;
#17985 = ORIENTED_EDGE ( 'NONE', *, *, #2903, .F. ) ;
#17986 = DIRECTION ( 'NONE',  ( -0.1566598588826321192, 0.9876526153536342445, 7.798540720466730171E-17 ) ) ;
#17987 = ORIENTED_EDGE ( 'NONE', *, *, #1733, .T. ) ;
#17988 = FACE_OUTER_BOUND ( 'NONE', #17195, .T. ) ;
#17989 = CARTESIAN_POINT ( 'NONE',  ( -29.21749237908259644, -82.58968536893641499, -17.32050807568878525 ) ) ;
#17990 = DIRECTION ( 'NONE',  ( 0.000000000000000000, 0.000000000000000000, 1.000000000000000000 ) ) ;
#17991 = ADVANCED_FACE ( 'NONE', ( #10548 ), #14915, .F. ) ;
#17992 = VERTEX_POINT ( 'NONE', #10723 ) ;
#17993 = EDGE_CURVE ( 'NONE', #3138, #14747, #1162, .T. ) ;
#17994 = VECTOR ( 'NONE', #7957, 1000.000000000000000 ) ;
#17995 = EDGE_CURVE ( 'NONE', #5108, #11461, #3532, .T. ) ;
#17996 = CARTESIAN_POINT ( 'NONE',  ( -72.50948914387967648, -26.68861478777332863, 4.330127018922218518 ) ) ;
#17997 = DIRECTION ( 'NONE',  ( 0.000000000000000000, 0.000000000000000000, 1.000000000000000000 ) ) ;
#17998 = DIRECTION ( 'NONE',  ( -0.9876526153536336894, -0.1566598588826349503, 0.000000000000000000 ) ) ;
#17999 = CARTESIAN_POINT ( 'NONE',  ( 1.399738696879940791, -77.73322974357483872, 4.330127018922209636 ) ) ;
#18000 = VERTEX_POINT ( 'NONE', #13391 ) ;
#18001 = VERTEX_POINT ( 'NONE', #16447 ) ;
#18002 = DIRECTION ( 'NONE',  ( -0.1566598588826321192, 0.9876526153536342445, 7.798540720466730171E-17 ) ) ;
#18003 = VERTEX_POINT ( 'NONE', #11939 ) ;
#18004 = VERTEX_POINT ( 'NONE', #7721 ) ;
#18005 = CARTESIAN_POINT ( 'NONE',  ( -55.42992169613162190, -29.04199019297804085, 12.99038105676661736 ) ) ;
#18006 = VERTEX_POINT ( 'NONE', #6494 ) ;
#18007 = DIRECTION ( 'NONE',  ( -1.000000000000000000, 0.000000000000000000, 0.000000000000000000 ) ) ;
#18008 = DIRECTION ( 'NONE',  ( -0.1566598588826321747, 0.9876526153536343555, 0.000000000000000000 ) ) ;
#18009 = VERTEX_POINT ( 'NONE', #713 ) ;
#18010 = CARTESIAN_POINT ( 'NONE',  ( -81.73462711737164454, 33.01666666666666572, 35.00000000000000000 ) ) ;
#18011 = CARTESIAN_POINT ( 'NONE',  ( -30.69897130211304770, -82.82467515726037277, -17.32050807568878525 ) ) ;
#18012 = EDGE_LOOP ( 'NONE', ( #18087, #4661 ) ) ;
#18013 = FACE_OUTER_BOUND ( 'NONE', #8653, .T. ) ;
#18014 = DIRECTION ( 'NONE',  ( 0.1856185419698760941, -0.9826218788918640312, 0.000000000000000000 ) ) ;
#18015 = ORIENTED_EDGE ( 'NONE', *, *, #17101, .T. ) ;
#18016 = CARTESIAN_POINT ( 'NONE',  ( -67.07739975943471222, -25.82698556391884992, -17.32050807568878170 ) ) ;
#18017 = FACE_OUTER_BOUND ( 'NONE', #8031, .T. ) ;
#18018 = CYLINDRICAL_SURFACE ( 'NONE', #3784, 1.500000000000001554 ) ;
#18019 = FACE_BOUND ( 'NONE', #6096, .T. ) ;
#18020 = CARTESIAN_POINT ( 'NONE',  ( -6.830590222863280658, -16.27073417207831696, 12.99038105676661026 ) ) ;
#18021 = CYLINDRICAL_SURFACE ( 'NONE', #1822, 1.500000000000001554 ) ;
#18022 = CARTESIAN_POINT ( 'NONE',  ( -53.94844277310118486, -28.80700040465408662, -4.330127018922181215 ) ) ;
#18024 = ORIENTED_EDGE ( 'NONE', *, *, #13156, .T. ) ;
#18023 = DIRECTION ( 'NONE',  ( 0.000000000000000000, 1.000000000000000000, -0.000000000000000000 ) ) ;
#18025 = EDGE_CURVE ( 'NONE', #16064, #4400, #3515, .T. ) ;
#18026 = ADVANCED_FACE ( 'NONE', ( #12231 ), #6214, .F. ) ;
#18027 = CARTESIAN_POINT ( 'NONE',  ( 3.231158466157551423, 19.73726462726227737, 35.00000000000000000 ) ) ;
#18028 = DIRECTION ( 'NONE',  ( -0.1566598588826321192, 0.9876526153536342445, 7.798540720466730171E-17 ) ) ;
#18029 = CIRCLE ( 'NONE', #13440, 1.500000000000000444 ) ;
#18030 = ORIENTED_EDGE ( 'NONE', *, *, #8697, .F. ) ;
#18031 = ORIENTED_EDGE ( 'NONE', *, *, #8467, .T. ) ;
#18032 = LINE ( 'NONE', #15241, #16403 ) ;
#18033 = ORIENTED_EDGE ( 'NONE', *, *, #8262, .F. ) ;
#18034 = DIRECTION ( 'NONE',  ( -0.1566598588826321192, 0.9876526153536342445, 7.798540720466730171E-17 ) ) ;
#18035 = DIRECTION ( 'NONE',  ( -0.9876526153536336894, -0.1566598588826349503, 0.000000000000000000 ) ) ;
#18036 = DIRECTION ( 'NONE',  ( -0.1566598588826321747, 0.9876526153536343555, 0.000000000000000000 ) ) ;
#18037 = DIRECTION ( 'NONE',  ( 1.000000000000000000, 0.000000000000000000, 0.000000000000000000 ) ) ;
#18038 = UNCERTAINTY_MEASURE_WITH_UNIT (LENGTH_MEASURE( 1.000000000000000082E-05 ), #13334, 'distance_accuracy_value', 'NONE');
#18039 = DIRECTION ( 'NONE',  ( -0.9876526153536341335, -0.1566598588826327021, 0.000000000000000000 ) ) ;
#18040 = AXIS2_PLACEMENT_3D ( 'NONE', #10012, #7876, #9913 ) ;
#18041 = ORIENTED_EDGE ( 'NONE', *, *, #14992, .F. ) ;
#18042 = FACE_OUTER_BOUND ( 'NONE', #15872, .T. ) ;
#18043 = ORIENTED_EDGE ( 'NONE', *, *, #17929, .F. ) ;
#18044 = DIRECTION ( 'NONE',  ( -0.1566598588826321747, 0.9876526153536343555, 0.000000000000000000 ) ) ;
#18045 = DIRECTION ( 'NONE',  ( -0.9876526153536341335, -0.1566598588826327021, 0.000000000000000000 ) ) ;
#18046 = CARTESIAN_POINT ( 'NONE',  ( -63.62061560569701157, -25.27867605782964588, 8.660254037844417496 ) ) ;
#18047 = EDGE_CURVE ( 'NONE', #3060, #4754, #7796, .T. ) ;
#18048 = CARTESIAN_POINT ( 'NONE',  ( -105.1664215174088213, -37.48287248576487940, -2.500000000000000000 ) ) ;
#18049 = VERTEX_POINT ( 'NONE', #15007 ) ;
#18050 = ORIENTED_EDGE ( 'NONE', *, *, #11615, .T. ) ;
#18051 = FACE_OUTER_BOUND ( 'NONE', #18117, .T. ) ;
#18052 = EDGE_CURVE ( 'NONE', #8214, #5148, #8405, .T. ) ;
#18053 = AXIS2_PLACEMENT_3D ( 'NONE', #8006, #2038, #9054 ) ;
#18054 = FACE_BOUND ( 'NONE', #11842, .T. ) ;
#18055 = DIRECTION ( 'NONE',  ( -0.1566598588826321192, 0.9876526153536342445, 7.798540720466730171E-17 ) ) ;
#18056 = ORIENTED_EDGE ( 'NONE', *, *, #564, .T. ) ;
#18057 = CARTESIAN_POINT ( 'NONE',  ( -7.034943543803747090, -21.36565710772908488, 8.660254037844413944 ) ) ;
#18058 = ORIENTED_EDGE ( 'NONE', *, *, #2766, .T. ) ;
#18059 = FACE_OUTER_BOUND ( 'NONE', #9234, .T. ) ;
#18060 = VECTOR ( 'NONE', #18295, 1000.000000000000000 ) ;
#18061 = LINE ( 'NONE', #5023, #17281 ) ;
#18062 = DIRECTION ( 'NONE',  ( -0.000000000000000000, -0.000000000000000000, -1.000000000000000000 ) ) ;
#18063 = DIRECTION ( 'NONE',  ( -0.9876526153536341335, 0.1566598588826326743, -0.000000000000000000 ) ) ;
#18064 = ORIENTED_EDGE ( 'NONE', *, *, #11895, .F. ) ;
#18065 = ORIENTED_EDGE ( 'NONE', *, *, #5243, .T. ) ;
#18066 = DIRECTION ( 'NONE',  ( 2.671473304378624222E-16, 0.000000000000000000, 1.000000000000000000 ) ) ;
#18067 = CARTESIAN_POINT ( 'NONE',  ( -71.23236354178970942, -31.54854793510013877, 17.32050807568881723 ) ) ;
#18068 = LINE ( 'NONE', #16627, #5697 ) ;
#18069 = ORIENTED_EDGE ( 'NONE', *, *, #7358, .F. ) ;
#18070 = CARTESIAN_POINT ( 'NONE',  ( -78.43540483600145308, -27.62857394106911713, 1.908195823574487804E-14 ) ) ;
#18071 = VECTOR ( 'NONE', #16057, 1000.000000000000000 ) ;
#18072 = ADVANCED_FACE ( 'NONE', ( #13472 ), #6117, .F. ) ;
#18073 = DIRECTION ( 'NONE',  ( -0.1566598588826321192, 0.9876526153536342445, 7.798540720466730171E-17 ) ) ;
#18074 = CARTESIAN_POINT ( 'NONE',  ( -172.2963380567813942, 56.58533696229243048, -2.499999999999999556 ) ) ;
#18075 = VERTEX_POINT ( 'NONE', #10650 ) ;
#18076 = CIRCLE ( 'NONE', #9870, 1.500000000000001332 ) ;
#18077 = EDGE_CURVE ( 'NONE', #968, #8399, #1448, .T. ) ;
#18078 = CYLINDRICAL_SURFACE ( 'NONE', #8800, 29.12282187559192437 ) ;
#18079 = CARTESIAN_POINT ( 'NONE',  ( -59.79999999999999716, 0.000000000000000000, 25.00000000000000000 ) ) ;
#18080 = LINE ( 'NONE', #16645, #12957 ) ;
#18081 = SHAPE_DEFINITION_REPRESENTATION ( #1964, #7353 ) ;
#18082 = DIRECTION ( 'NONE',  ( -0.9876526153536336894, -0.1566598588826349503, 0.000000000000000000 ) ) ;
#18083 = CARTESIAN_POINT ( 'NONE',  ( -25.26688191766805858, -81.96304593340589406, -12.99038105676658539 ) ) ;
#18084 = DIRECTION ( 'NONE',  ( -0.000000000000000000, -0.000000000000000000, -1.000000000000000000 ) ) ;
#18085 = DIRECTION ( 'NONE',  ( -0.1566598588826321192, 0.9876526153536342445, 7.798540720466730171E-17 ) ) ;
#18086 = DIRECTION ( 'NONE',  ( -0.9876526153536336894, -0.1566598588826350336, 0.000000000000000000 ) ) ;
#18087 = ORIENTED_EDGE ( 'NONE', *, *, #4064, .F. ) ;
#18088 = ORIENTED_EDGE ( 'NONE', *, *, #6482, .F. ) ;
#18089 = DIRECTION ( 'NONE',  ( 2.735665993912342121E-16, 0.000000000000000000, 1.000000000000000000 ) ) ;
#18090 = AXIS2_PLACEMENT_3D ( 'NONE', #5078, #11045, #15229 ) ;
#18091 = FACE_OUTER_BOUND ( 'NONE', #12972, .T. ) ;
#18092 = VERTEX_POINT ( 'NONE', #15095 ) ;
#18093 = VERTEX_POINT ( 'NONE', #4863 ) ;
#18094 = ORIENTED_EDGE ( 'NONE', *, *, #17129, .F. ) ;
#18095 = AXIS2_PLACEMENT_3D ( 'NONE', #17251, #12936, #10378 ) ;
#18096 = EDGE_CURVE ( 'NONE', #7506, #8207, #10799, .T. ) ;
#18097 = ADVANCED_FACE ( 'NONE', ( #3155 ), #17982, .F. ) ;
#18098 = AXIS2_PLACEMENT_3D ( 'NONE', #12689, #18547, #5518 ) ;
#18099 = DIRECTION ( 'NONE',  ( 0.000000000000000000, 0.000000000000000000, 1.000000000000000000 ) ) ;
#18100 = EDGE_CURVE ( 'NONE', #1829, #16999, #12619, .T. ) ;
#18101 = DIRECTION ( 'NONE',  ( 0.000000000000000000, 0.000000000000000000, 1.000000000000000000 ) ) ;
#18102 = EDGE_CURVE ( 'NONE', #16138, #14196, #9002, .T. ) ;
#18103 = DIRECTION ( 'NONE',  ( -0.1566598588826321747, 0.9876526153536343555, 0.000000000000000000 ) ) ;
#18104 = MECHANICAL_DESIGN_GEOMETRIC_PRESENTATION_REPRESENTATION (  '', ( #13213 ), #3226 ) ;
#18105 = DIRECTION ( 'NONE',  ( -0.1566598588826321192, 0.9876526153536342445, 7.798540720466730171E-17 ) ) ;
#18106 = FILL_AREA_STYLE ('',( #8022 ) ) ;
#18107 = CIRCLE ( 'NONE', #17793, 1.500000000000000888 ) ;
#18108 = ORIENTED_EDGE ( 'NONE', *, *, #15843, .F. ) ;
#18109 = DIRECTION ( 'NONE',  ( -0.1566598588826321747, 0.9876526153536343555, 0.000000000000000000 ) ) ;
#18110 = VERTEX_POINT ( 'NONE', #9040 ) ;
#18111 = DIRECTION ( 'NONE',  ( 0.000000000000000000, 0.000000000000000000, 1.000000000000000000 ) ) ;
#18112 = FACE_BOUND ( 'NONE', #12358, .T. ) ;
#18113 = CIRCLE ( 'NONE', #9902, 1.500000000000001332 ) ;
#18114 = CYLINDRICAL_SURFACE ( 'NONE', #16600, 1.500000000000001554 ) ;
#18115 = CARTESIAN_POINT ( 'NONE',  ( -64.60826822105062206, -25.43533591671228677, 21.65063509461101887 ) ) ;
#18117 = EDGE_LOOP ( 'NONE', ( #7717, #11751, #9596, #4789 ) ) ;
#18116 = CARTESIAN_POINT ( 'NONE',  ( -75.18297400320422241, -32.17518737063066681, 4.330127018922217630 ) ) ;
#18118 = CARTESIAN_POINT ( 'NONE',  ( -12.46703292824873088, -22.22728633158356359, -12.99038105676658006 ) ) ;
#18119 = EDGE_LOOP ( 'NONE', ( #6579, #7501, #3023, #3519, #11738, #14064, #12009, #17584, #6809, #14773 ) ) ;
#18120 = AXIS2_PLACEMENT_3D ( 'NONE', #11865, #13572, #517 ) ;
#18122 = ORIENTED_EDGE ( 'NONE', *, *, #5318, .F. ) ;
#18121 = EDGE_CURVE ( 'NONE', #8348, #5828, #1843, .T. ) ;
#18123 = EDGE_LOOP ( 'NONE', ( #16133, #6291, #18204, #17310 ) ) ;
#18124 = DIRECTION ( 'NONE',  ( -0.9876526153536341335, -0.1566598588826327021, 0.000000000000000000 ) ) ;
#18125 = EDGE_CURVE ( 'NONE', #3927, #3563, #11991, .T. ) ;
#18126 = FACE_OUTER_BOUND ( 'NONE', #7001, .T. ) ;
#18127 = ORIENTED_EDGE ( 'NONE', *, *, #16833, .T. ) ;
#18128 = CARTESIAN_POINT ( 'NONE',  ( 0.000000000000000000, 0.000000000000000000, 30.00000000000000000 ) ) ;
#18129 = CARTESIAN_POINT ( 'NONE',  ( -129.1404785418517918, 8.737237296935983721, -5.316127001577083178 ) ) ;
#18130 = PRODUCT_RELATED_PRODUCT_CATEGORY ( 'part', '', ( #18543 ) ) ;
#18131 = DIRECTION ( 'NONE',  ( -0.1566598588826321192, 0.9876526153536342445, 7.798540720466730171E-17 ) ) ;
#18132 = CARTESIAN_POINT ( 'NONE',  ( -73.70149508017377116, -31.94019758230671258, 12.99038105676661736 ) ) ;
#18133 = CARTESIAN_POINT ( 'NONE',  ( -79.94364498743971126, 2.107449674570485154, -2.869442248077125779 ) ) ;
#18134 = EDGE_CURVE ( 'NONE', #17191, #8885, #10515, .T. ) ;
#18135 = CARTESIAN_POINT ( 'NONE',  ( -126.9542992265479739, -15.29553669137375671, -2.584671478510880416 ) ) ;
#18136 = DIRECTION ( 'NONE',  ( 1.000000000000000000, -3.469446951953611033E-15, 0.000000000000000000 ) ) ;
#18137 = DIRECTION ( 'NONE',  ( 0.000000000000000000, 0.000000000000000000, 1.000000000000000000 ) ) ;
#18138 = ORIENTED_EDGE ( 'NONE', *, *, #16117, .F. ) ;
#18139 = CIRCLE ( 'NONE', #11713, 1.500000000000001332 ) ;
#18140 = CARTESIAN_POINT ( 'NONE',  ( -7.528769851480577202, -21.44398703717040888, 12.99038105676661026 ) ) ;
#18141 = DIRECTION ( 'NONE',  ( -0.9876526153536341335, -0.1566598588826327021, 0.000000000000000000 ) ) ;
#18142 = DIRECTION ( 'NONE',  ( -0.9876526153536341335, -0.1566598588826327021, 0.000000000000000000 ) ) ;
#18143 = EDGE_LOOP ( 'NONE', ( #4899, #14030, #2000, #15349 ) ) ;
#18144 = CARTESIAN_POINT ( 'NONE',  ( -2.000000000000000000, 2.449293598294706414E-16, -40.65685424949239035 ) ) ;
#18145 = AXIS2_PLACEMENT_3D ( 'NONE', #15091, #2117, #2387 ) ;
#18146 = EDGE_LOOP ( 'NONE', ( #14002, #17455 ) ) ;
#18147 = ORIENTED_EDGE ( 'NONE', *, *, #3692, .F. ) ;
#18148 = ORIENTED_EDGE ( 'NONE', *, *, #11094, .F. ) ;
#18149 = ORIENTED_EDGE ( 'NONE', *, *, #11014, .T. ) ;
#18150 = DIRECTION ( 'NONE',  ( 0.000000000000000000, 0.000000000000000000, 1.000000000000000000 ) ) ;
#18151 = AXIS2_PLACEMENT_3D ( 'NONE', #15248, #3761, #9281 ) ;
#18152 = AXIS2_PLACEMENT_3D ( 'NONE', #8281, #6862, #18167 ) ;
#18153 = ORIENTED_EDGE ( 'NONE', *, *, #304, .T. ) ;
#18154 = FACE_BOUND ( 'NONE', #13347, .T. ) ;
#18155 =( GEOMETRIC_REPRESENTATION_CONTEXT ( 3 ) GLOBAL_UNCERTAINTY_ASSIGNED_CONTEXT ( ( #6981 ) ) GLOBAL_UNIT_ASSIGNED_CONTEXT ( ( #18508, #14084, #7943 ) ) REPRESENTATION_CONTEXT ( 'NONE', 'WORKASPACE' ) );
#18156 = CARTESIAN_POINT ( 'NONE',  ( -77.65210554158829837, -32.56683701783724416, 1.869203119972154228E-14 ) ) ;
#18157 = EDGE_CURVE ( 'NONE', #16131, #4419, #230, .T. ) ;
#18158 = CIRCLE ( 'NONE', #13258, 1.500000000000000444 ) ;
#18159 = ADVANCED_FACE ( 'NONE', ( #5248 ), #15197, .F. ) ;
#18160 = ORIENTED_EDGE ( 'NONE', *, *, #6948, .F. ) ;
#18161 = VECTOR ( 'NONE', #13143, 1000.000000000000000 ) ;
#18162 = EDGE_CURVE ( 'NONE', #16065, #15050, #6685, .T. ) ;
#18163 = DIRECTION ( 'NONE',  ( -0.1566598588826321192, 0.9876526153536342445, 7.798540720466730171E-17 ) ) ;
#18164 = AXIS2_PLACEMENT_3D ( 'NONE', #10685, #14953, #2065 ) ;
#18165 = EDGE_LOOP ( 'NONE', ( #10492, #8074 ) ) ;
#18166 = DIRECTION ( 'NONE',  ( -0.1566598588826321192, 0.9876526153536342445, 7.798540720466730171E-17 ) ) ;
#18167 = DIRECTION ( 'NONE',  ( -0.9876526153536336894, -0.1566598588826349503, 0.000000000000000000 ) ) ;
#18168 = CARTESIAN_POINT ( 'NONE',  ( -67.77557938805200877, -31.00023842901093118, -8.660254037844380193 ) ) ;
#18169 = ORIENTED_EDGE ( 'NONE', *, *, #13307, .F. ) ;
#18170 = EDGE_LOOP ( 'NONE', ( #4495, #10764, #9610, #1310 ) ) ;
#18171 = CARTESIAN_POINT ( 'NONE',  ( 0.000000000000000000, 0.000000000000000000, -37.00000000000000711 ) ) ;
#18172 = CARTESIAN_POINT ( 'NONE',  ( -68.55887868246516348, -26.06197535224280060, 1.908195823574487804E-14 ) ) ;
#18173 = EDGE_LOOP ( 'NONE', ( #18638, #9498 ) ) ;
#18174 = CIRCLE ( 'NONE', #10842, 5.000000000000004441 ) ;
#18175 = ORIENTED_EDGE ( 'NONE', *, *, #12985, .F. ) ;
#18176 = DIRECTION ( 'NONE',  ( -0.9876526153536336894, -0.1566598588826349503, 0.000000000000000000 ) ) ;
#18177 = ORIENTED_EDGE ( 'NONE', *, *, #18655, .F. ) ;
#18178 = AXIS2_PLACEMENT_3D ( 'NONE', #5226, #15352, #877 ) ;
#18179 = EDGE_LOOP ( 'NONE', ( #7786, #5921, #3920, #8395 ) ) ;
#18180 = CARTESIAN_POINT ( 'NONE',  ( -129.1404785418518202, -14.43864122329464195, 5.316127001577084066 ) ) ;
#18181 = CIRCLE ( 'NONE', #9958, 1.500000000000000888 ) ;
#18182 = ORIENTED_EDGE ( 'NONE', *, *, #23, .F. ) ;
#18183 = VECTOR ( 'NONE', #1202, 1000.000000000000000 ) ;
#18184 = VECTOR ( 'NONE', #16115, 1000.000000000000000 ) ;
#18185 = CIRCLE ( 'NONE', #9963, 1.500000000000000444 ) ;
#18186 = FACE_BOUND ( 'NONE', #12121, .T. ) ;
#18187 = FACE_OUTER_BOUND ( 'NONE', #5647, .T. ) ;
#18188 = LINE ( 'NONE', #6787, #9026 ) ;
#18189 = FILL_AREA_STYLE ('',( #10658 ) ) ;
#18190 = CIRCLE ( 'NONE', #615, 1.500000000000000888 ) ;
#18191 = AXIS2_PLACEMENT_3D ( 'NONE', #936, #18307, #8218 ) ;
#18192 = EDGE_CURVE ( 'NONE', #10083, #10544, #2787, .T. ) ;
#18193 = LINE ( 'NONE', #16937, #605 ) ;
#18195 = DIRECTION ( 'NONE',  ( -0.1566598588826321192, 0.9876526153536342445, 7.798540720466730171E-17 ) ) ;
#18194 = AXIS2_PLACEMENT_3D ( 'NONE', #3507, #3882, #9707 ) ;
#18196 = ORIENTED_EDGE ( 'NONE', *, *, #12149, .T. ) ;
#18197 = LINE ( 'NONE', #5170, #12989 ) ;
#18198 = CARTESIAN_POINT ( 'NONE',  ( -37.61253960958845255, -83.92129416943878084, -17.32050807568878525 ) ) ;
#18199 = AXIS2_PLACEMENT_3D ( 'NONE', #13400, #4875, #4682 ) ;
#18200 = VERTEX_POINT ( 'NONE', #18278 ) ;
#18201 = EDGE_LOOP ( 'NONE', ( #9163, #12896, #1955, #13019 ) ) ;
#18202 = APPLICATION_CONTEXT ( 'automotive_design' ) ;
#18203 = DIRECTION ( 'NONE',  ( -0.9876526153536344665, -0.1566598588826304539, 0.000000000000000000 ) ) ;
#18204 = ORIENTED_EDGE ( 'NONE', *, *, #17274, .T. ) ;
#18205 = AXIS2_PLACEMENT_3D ( 'NONE', #4698, #4424, #10304 ) ;
#18206 = ORIENTED_EDGE ( 'NONE', *, *, #10634, .T. ) ;
#18207 = EDGE_CURVE ( 'NONE', #3520, #98, #2652, .T. ) ;
#18208 = ORIENTED_EDGE ( 'NONE', *, *, #8341, .T. ) ;
#18209 = DIRECTION ( 'NONE',  ( -0.9876526153536336894, -0.1566598588826349503, 0.000000000000000000 ) ) ;
#18210 = DIRECTION ( 'NONE',  ( -0.9876526153536341335, -0.1566598588826327021, 0.000000000000000000 ) ) ;
#18211 = EDGE_LOOP ( 'NONE', ( #11812, #10237 ) ) ;
#18212 = VECTOR ( 'NONE', #15231, 1000.000000000000000 ) ;
#18213 = CARTESIAN_POINT ( 'NONE',  ( -7.034943543803747090, -21.36565710772908488, -17.32050807568878170 ) ) ;
#18214 = ORIENTED_EDGE ( 'NONE', *, *, #3792, .F. ) ;
#18215 = AXIS2_PLACEMENT_3D ( 'NONE', #9789, #16726, #5330 ) ;
#18216 = DIRECTION ( 'NONE',  ( -0.1566598588826321192, 0.9876526153536342445, 7.798540720466731404E-17 ) ) ;
#18217 = CARTESIAN_POINT ( 'NONE',  ( 73.09088021254186174, 1.387778780781445676E-14, 7.500000000000000000 ) ) ;
#18218 = AXIS2_PLACEMENT_3D ( 'NONE', #6545, #4992, #1897 ) ;
#18219 = DIRECTION ( 'NONE',  ( -0.1566598588826321192, 0.9876526153536342445, 7.798540720466731404E-17 ) ) ;
#18220 = EDGE_LOOP ( 'NONE', ( #15367, #3013, #16503, #7760 ) ) ;
#18221 = CARTESIAN_POINT ( 'NONE',  ( -40.61513246582718040, -26.69209230973856251, 12.99038105676661736 ) ) ;
#18222 = VERTEX_POINT ( 'NONE', #12611 ) ;
#18223 = CYLINDRICAL_SURFACE ( 'NONE', #3503, 1.500000000000001554 ) ;
#18224 = DIRECTION ( 'NONE',  ( -0.9876526153536336894, -0.1566598588826349503, 0.000000000000000000 ) ) ;
#18225 = PLANE ( 'NONE',  #16075 ) ;
#18226 = EDGE_CURVE ( 'NONE', #9762, #8333, #9713, .T. ) ;
#18227 = AXIS2_PLACEMENT_3D ( 'NONE', #14745, #13593, #1762 ) ;
#18229 = VERTEX_POINT ( 'NONE', #5033 ) ;
#18228 = CARTESIAN_POINT ( 'NONE',  ( -136.4286012789710867, -132.1908753210555574, 2.500000000000000000 ) ) ;
#18230 = ADVANCED_FACE ( 'NONE', ( #13751 ), #3709, .F. ) ;
#18231 = CARTESIAN_POINT ( 'NONE',  ( 73.09088021254186174, 1.387778780781445676E-14, 19.99999999999997513 ) ) ;
#18232 = AXIS2_PLACEMENT_3D ( 'NONE', #367, #8891, #7471 ) ;
#18233 = CYLINDRICAL_SURFACE ( 'NONE', #941, 1.500000000000001554 ) ;
#18234 = ORIENTED_EDGE ( 'NONE', *, *, #4912, .F. ) ;
#18235 = EDGE_LOOP ( 'NONE', ( #9338, #6210 ) ) ;
#18236 = CARTESIAN_POINT ( 'NONE',  ( -64.20000000000000284, 2.694222958124175527E-16, -20.00000000000000000 ) ) ;
#18237 = VECTOR ( 'NONE', #9905, 1000.000000000000000 ) ;
#18238 = DIRECTION ( 'NONE',  ( -0.1566598588826321192, 0.9876526153536342445, 7.798540720466730171E-17 ) ) ;
#18239 = AXIS2_PLACEMENT_3D ( 'NONE', #9737, #2519, #12630 ) ;
#18240 = CARTESIAN_POINT ( 'NONE',  ( -128.1659926135409933, 9.451401928990495804, -3.278196957010496959 ) ) ;
#18241 = ORIENTED_EDGE ( 'NONE', *, *, #2967, .T. ) ;
#18242 = CARTESIAN_POINT ( 'NONE',  ( -10.45209268736360997, -79.61314805016641571, -4.330127018922185655 ) ) ;
#18243 = DIRECTION ( 'NONE',  ( -0.1566598588826321192, 0.9876526153536342445, 7.798540720466731404E-17 ) ) ;
#18244 = CARTESIAN_POINT ( 'NONE',  ( -79.05438463828195950, 1.499069270643396345, -3.389939594122236333 ) ) ;
#18245 = CIRCLE ( 'NONE', #5183, 1.500000000000000888 ) ;
#18246 = CARTESIAN_POINT ( 'NONE',  ( 55.85952145814821534, 6.938893903907228378E-15, -30.00000000000000000 ) ) ;
#18247 = CARTESIAN_POINT ( 'NONE',  ( -71.72618984946653597, -31.62687786454144856, -4.330127018922181215 ) ) ;
#18248 = DIRECTION ( 'NONE',  ( -0.9826218788918642533, -0.1856185419698762884, 0.000000000000000000 ) ) ;
#18249 = DIRECTION ( 'NONE',  ( -1.000000000000000000, 0.000000000000000000, 0.000000000000000000 ) ) ;
#18250 = EDGE_CURVE ( 'NONE', #3501, #2218, #18068, .T. ) ;
#18251 = ORIENTED_EDGE ( 'NONE', *, *, #2059, .T. ) ;
#18252 = VECTOR ( 'NONE', #15010, 1000.000000000000000 ) ;
#18253 = EDGE_CURVE ( 'NONE', #8678, #9632, #11105, .T. ) ;
#18254 = DIRECTION ( 'NONE',  ( -0.1566598588826321192, 0.9876526153536342445, 7.798540720466730171E-17 ) ) ;
#18255 = CARTESIAN_POINT ( 'NONE',  ( -12.46703292824872733, -22.22728633158356359, 21.65063509461101177 ) ) ;
#18256 = VECTOR ( 'NONE', #16271, 1000.000000000000000 ) ;
#18257 = AXIS2_PLACEMENT_3D ( 'NONE', #86, #12864, #14102 ) ;
#18258 = CARTESIAN_POINT ( 'NONE',  ( -110.7369027592740167, -34.07064978273316314, 2.500000000000000000 ) ) ;
#18259 = ORIENTED_EDGE ( 'NONE', *, *, #17837, .F. ) ;
#18260 = ORIENTED_EDGE ( 'NONE', *, *, #1223, .T. ) ;
#18261 = DIRECTION ( 'NONE',  ( -0.1566598588826321192, 0.9876526153536342445, 7.798540720466730171E-17 ) ) ;
#18262 = FACE_BOUND ( 'NONE', #18211, .T. ) ;
#18263 = VECTOR ( 'NONE', #11652, 1000.000000000000000 ) ;
#18264 = DIRECTION ( 'NONE',  ( -0.1566598588826321192, 0.9876526153536342445, 7.798540720466730171E-17 ) ) ;
#18265 = VECTOR ( 'NONE', #8582, 1000.000000000000000 ) ;
#18266 = DIRECTION ( 'NONE',  ( 0.000000000000000000, 0.000000000000000000, 1.000000000000000000 ) ) ;
#18267 = DIRECTION ( 'NONE',  ( -0.1566598588826321192, 0.9876526153536342445, 7.798540720466730171E-17 ) ) ;
#18268 = ORIENTED_EDGE ( 'NONE', *, *, #6465, .T. ) ;
#18269 = VECTOR ( 'NONE', #15035, 1000.000000000000000 ) ;
#18270 = DIRECTION ( 'NONE',  ( 0.000000000000000000, 0.000000000000000000, 1.000000000000000000 ) ) ;
#18271 = PLANE ( 'NONE',  #289 ) ;
#18272 = CARTESIAN_POINT ( 'NONE',  ( -32.50955822205765600, -20.34389050302675628, 17.32050807568881723 ) ) ;
#18273 = CARTESIAN_POINT ( 'NONE',  ( -70.00000000000000000, 44.99999999999999289, 20.00000000000002132 ) ) ;
#18274 = ORIENTED_EDGE ( 'NONE', *, *, #14993, .T. ) ;
#18275 = CARTESIAN_POINT ( 'NONE',  ( -64.60826822105063627, -25.43533591671227256, -12.99038105676658006 ) ) ;
#18276 = FACE_OUTER_BOUND ( 'NONE', #778, .T. ) ;
#18277 = EDGE_CURVE ( 'NONE', #7282, #18001, #12931, .T. ) ;
#18278 = CARTESIAN_POINT ( 'NONE',  ( -7.818242838216901802, -16.42739403096095074, -17.32050807568878170 ) ) ;
#18279 = CIRCLE ( 'NONE', #14595, 1.500000000000000888 ) ;
#18280 = ORIENTED_EDGE ( 'NONE', *, *, #5464, .T. ) ;
#18281 = EDGE_LOOP ( 'NONE', ( #2516, #6537, #12712, #10410 ) ) ;
#18282 = CYLINDRICAL_SURFACE ( 'NONE', #16394, 1.500000000000001554 ) ;
#18283 = EDGE_CURVE ( 'NONE', #14582, #356, #10200, .T. ) ;
#18284 = DIRECTION ( 'NONE',  ( -0.1566598588826321192, 0.9876526153536342445, 7.798540720466731404E-17 ) ) ;
#18285 = CARTESIAN_POINT ( 'NONE',  ( -169.7748756787665059, 31.94743695617602341, 3.563338245596213039 ) ) ;
#18286 = STYLED_ITEM ( 'NONE', ( #12311 ), #8769 ) ;
#18287 = AXIS2_PLACEMENT_3D ( 'NONE', #15593, #2617, #9907 ) ;
#18288 = CARTESIAN_POINT ( 'NONE',  ( -42.09661138885763876, -26.92708209806250608, -21.65063509461098334 ) ) ;
#18289 = DIRECTION ( 'NONE',  ( 0.000000000000000000, 0.000000000000000000, 1.000000000000000000 ) ) ;
#18290 = CARTESIAN_POINT ( 'NONE',  ( -72.31226064957499489, 45.98387735189907488, 3.156966122918108741 ) ) ;
#18291 = CARTESIAN_POINT ( 'NONE',  ( 0.000000000000000000, 0.000000000000000000, 0.000000000000000000 ) ) ;
#18292 = LINE ( 'NONE', #9807, #16654 ) ;
#18293 = CARTESIAN_POINT ( 'NONE',  ( -3.578159390066044665, -20.81734760163988440, -8.660254037844383745 ) ) ;
#18294 = DIRECTION ( 'NONE',  ( -0.9876526153536336894, -0.1566598588826350336, 0.000000000000000000 ) ) ;
#18295 = DIRECTION ( 'NONE',  ( -0.1566598588826321192, 0.9876526153536342445, 7.798540720466730171E-17 ) ) ;
#18296 = ORIENTED_EDGE ( 'NONE', *, *, #8696, .T. ) ;
#18297 = ORIENTED_EDGE ( 'NONE', *, *, #14004, .T. ) ;
#18298 = AXIS2_PLACEMENT_3D ( 'NONE', #9563, #10872, #762 ) ;
#18299 = FACE_BOUND ( 'NONE', #7413, .T. ) ;
#18300 = LINE ( 'NONE', #2318, #12103 ) ;
#18301 = VERTEX_POINT ( 'NONE', #5107 ) ;
#18302 = ORIENTED_EDGE ( 'NONE', *, *, #6271, .T. ) ;
#18303 = CARTESIAN_POINT ( 'NONE',  ( -10.78120068427780964, -16.89737360760884144, -8.660254037844380193 ) ) ;
#18304 = CARTESIAN_POINT ( 'NONE',  ( -21.64537945316773460, -18.62063205531779886, 21.65063509461101532 ) ) ;
#18305 = EDGE_CURVE ( 'NONE', #16372, #8304, #13848, .T. ) ;
#18306 = CARTESIAN_POINT ( 'NONE',  ( -41.56315007100294423, -84.54793360496933019, 21.65063509461101532 ) ) ;
#18307 = DIRECTION ( 'NONE',  ( -0.1566598588826321192, 0.9876526153536342445, 7.798540720466730171E-17 ) ) ;
#18308 = ORIENTED_EDGE ( 'NONE', *, *, #12332, .T. ) ;
#18309 = CYLINDRICAL_SURFACE ( 'NONE', #13321, 1.500000000000001554 ) ;
#18310 = CIRCLE ( 'NONE', #12190, 1.499999999999999556 ) ;
#18311 = DIRECTION ( 'NONE',  ( -0.000000000000000000, -0.000000000000000000, -1.000000000000000000 ) ) ;
#18312 = FACE_OUTER_BOUND ( 'NONE', #6288, .T. ) ;
#18313 = ORIENTED_EDGE ( 'NONE', *, *, #12052, .F. ) ;
#18314 = CARTESIAN_POINT ( 'NONE',  ( -75.96627329761737712, -27.23692429386254332, 12.99038105676661736 ) ) ;
#18315 = SURFACE_SIDE_STYLE ('',( #15516 ) ) ;
#18316 = EDGE_CURVE ( 'NONE', #15072, #16032, #15668, .T. ) ;
#18317 = CARTESIAN_POINT ( 'NONE',  ( -70.04035760549561473, -26.29696514056675483, 17.32050807568881723 ) ) ;
#18318 = ORIENTED_EDGE ( 'NONE', *, *, #10416, .T. ) ;
#18319 = CARTESIAN_POINT ( 'NONE',  ( -46.50141314777110324, -85.33123289938248490, 12.99038105676661203 ) ) ;
#18320 = VERTEX_POINT ( 'NONE', #16214 ) ;
#18321 = DIRECTION ( 'NONE',  ( -0.1566598588826321192, 0.9876526153536342445, 7.798540720466731404E-17 ) ) ;
#18322 = CARTESIAN_POINT ( 'NONE',  ( -47.32434745236209750, -22.69378838626623107, 17.32050807568881723 ) ) ;
#18323 = DIRECTION ( 'NONE',  ( -0.9876526153536344665, -0.1566598588826304539, 0.000000000000000000 ) ) ;
#18324 = EDGE_LOOP ( 'NONE', ( #11539, #10914 ) ) ;
#18325 = ORIENTED_EDGE ( 'NONE', *, *, #14558, .T. ) ;
#18326 = DIRECTION ( 'NONE',  ( -0.1566598588826321192, 0.9876526153536342445, 7.798540720466731404E-17 ) ) ;
#18327 = CIRCLE ( 'NONE', #6179, 1.500000000000000444 ) ;
#18328 = ORIENTED_EDGE ( 'NONE', *, *, #15531, .F. ) ;
#18329 = EDGE_LOOP ( 'NONE', ( #15470, #4449 ) ) ;
#18330 = CARTESIAN_POINT ( 'NONE',  ( -15.92381708198642798, -22.77559583767277473, -12.99038105676658006 ) ) ;
#18331 = EDGE_CURVE ( 'NONE', #17378, #5203, #14770, .T. ) ;
#18332 = ORIENTED_EDGE ( 'NONE', *, *, #17340, .F. ) ;
#18333 = DIRECTION ( 'NONE',  ( -0.1566598588826321192, 0.9876526153536342445, 7.798540720466731404E-17 ) ) ;
#18334 = ORIENTED_EDGE ( 'NONE', *, *, #4622, .F. ) ;
#18335 = DIRECTION ( 'NONE',  ( -0.000000000000000000, -0.000000000000000000, -1.000000000000000000 ) ) ;
#18336 = FACE_OUTER_BOUND ( 'NONE', #2993, .T. ) ;
#18337 = CARTESIAN_POINT ( 'NONE',  ( -128.8620198725179193, 9.173231832019821397, -4.223374618371430245 ) ) ;
#18338 = DIRECTION ( 'NONE',  ( -0.1566598588826321747, 0.9876526153536343555, 0.000000000000000000 ) ) ;
#18339 = DIRECTION ( 'NONE',  ( -0.9876526153536341335, -0.1566598588826327021, 0.000000000000000000 ) ) ;
#18340 = EDGE_CURVE ( 'NONE', #14985, #10067, #17221, .T. ) ;
#18341 = DIRECTION ( 'NONE',  ( 0.000000000000000000, 0.000000000000000000, 1.000000000000000000 ) ) ;
#18342 = DIRECTION ( 'NONE',  ( 0.000000000000000000, 0.000000000000000000, -1.000000000000000000 ) ) ;
#18343 = FACE_OUTER_BOUND ( 'NONE', #4722, .T. ) ;
#18344 = EDGE_CURVE ( 'NONE', #5655, #16506, #16287, .T. ) ;
#18345 = CARTESIAN_POINT ( 'NONE',  ( -126.3445361634317265, 9.599524378652860790, -2.499999999999999112 ) ) ;
#18346 = CYLINDRICAL_SURFACE ( 'NONE', #3493, 1.500000000000000666 ) ;
#18347 = DIRECTION ( 'NONE',  ( -0.1566598588826321192, 0.9876526153536342445, 7.798540720466731404E-17 ) ) ;
#18348 = DIRECTION ( 'NONE',  ( -0.1566598588826321192, 0.9876526153536342445, 7.798540720466730171E-17 ) ) ;
#18349 = ADVANCED_FACE ( 'NONE', ( #15063 ), #14974, .F. ) ;
#18350 = ORIENTED_EDGE ( 'NONE', *, *, #14564, .T. ) ;
#18351 = FACE_OUTER_BOUND ( 'NONE', #3111, .T. ) ;
#18352 = FACE_BOUND ( 'NONE', #5586, .T. ) ;
#18353 = EDGE_CURVE ( 'NONE', #5886, #1028, #9622, .T. ) ;
#18354 = ADVANCED_FACE ( 'NONE', ( #6374 ), #13718, .F. ) ;
#18355 = DIRECTION ( 'NONE',  ( -0.9876526153536344665, -0.1566598588826304539, 0.000000000000000000 ) ) ;
#18356 = CIRCLE ( 'NONE', #8630, 1.500000000000000888 ) ;
#18357 = ORIENTED_EDGE ( 'NONE', *, *, #16117, .T. ) ;
#18358 = EDGE_CURVE ( 'NONE', #17451, #13951, #395, .T. ) ;
#18359 = EDGE_CURVE ( 'NONE', #7684, #3359, #1754, .T. ) ;
#18360 = FACE_OUTER_BOUND ( 'NONE', #11934, .T. ) ;
#18361 = LINE ( 'NONE', #5332, #10865 ) ;
#18362 = CARTESIAN_POINT ( 'NONE',  ( -42.55080268635659735, -84.70459346385193555, -8.660254037844385522 ) ) ;
#18363 = DIRECTION ( 'NONE',  ( -0.1566598588826321747, 0.9876526153536343555, 0.000000000000000000 ) ) ;
#18364 = ORIENTED_EDGE ( 'NONE', *, *, #434, .T. ) ;
#18365 = CARTESIAN_POINT ( 'NONE',  ( 0.000000000000000000, 0.000000000000000000, -19.99999999999999645 ) ) ;
#18366 = AXIS2_PLACEMENT_3D ( 'NONE', #6794, #12626, #1110 ) ;
#18367 = CARTESIAN_POINT ( 'NONE',  ( -169.4934689854139549, 31.92509550690243003, -3.279750847804471903 ) ) ;
#18368 = ORIENTED_EDGE ( 'NONE', *, *, #7708, .T. ) ;
#18369 = ORIENTED_EDGE ( 'NONE', *, *, #9202, .F. ) ;
#18370 = DIRECTION ( 'NONE',  ( -0.1566598588826321192, 0.9876526153536342445, 7.798540720466730171E-17 ) ) ;
#18371 = VERTEX_POINT ( 'NONE', #16307 ) ;
#18372 = ORIENTED_EDGE ( 'NONE', *, *, #2489, .F. ) ;
#18373 = DIRECTION ( 'NONE',  ( -0.1566598588826321192, 0.9876526153536342445, 7.798540720466730171E-17 ) ) ;
#18374 = CARTESIAN_POINT ( 'NONE',  ( -170.2272147085104166, 32.06920008862883975, 4.223374618371441791 ) ) ;
#18375 = EDGE_CURVE ( 'NONE', #17370, #5722, #13536, .T. ) ;
#18376 = FACE_BOUND ( 'NONE', #6995, .T. ) ;
#18377 = CARTESIAN_POINT ( 'NONE',  ( -57.36559191666103175, -87.05449134709142811, 1.443110928631665584E-14 ) ) ;
#18378 = CARTESIAN_POINT ( 'NONE',  ( 6.744699544032231168E-15, -6.824871242521816123E-15, 20.00000000000000000 ) ) ;
#18379 = DIRECTION ( 'NONE',  ( 0.8974640438000611731, -0.4410876217783063491, 6.399844032197820264E-17 ) ) ;
#18380 = ADVANCED_FACE ( 'NONE', ( #18042 ), #4918, .F. ) ;
#18381 = ORIENTED_EDGE ( 'NONE', *, *, #11487, .F. ) ;
#18382 = ADVANCED_FACE ( 'NONE', ( #16592 ), #17756, .F. ) ;
#18383 = CARTESIAN_POINT ( 'NONE',  ( -129.1404785418517918, -15.35070196317932911, -2.500000000000000000 ) ) ;
#18384 = DIRECTION ( 'NONE',  ( -0.1566598588826321192, 0.9876526153536342445, 7.798540720466731404E-17 ) ) ;
#18385 = VERTEX_POINT ( 'NONE', #3577 ) ;
#18386 = DIRECTION ( 'NONE',  ( -1.000000000000000000, 0.000000000000000000, 0.000000000000000000 ) ) ;
#18387 = LINE ( 'NONE', #5361, #16840 ) ;
#18388 = VERTEX_POINT ( 'NONE', #679 ) ;
#18389 = VERTEX_POINT ( 'NONE', #15165 ) ;
#18390 = FACE_BOUND ( 'NONE', #2230, .T. ) ;
#18391 = CARTESIAN_POINT ( 'NONE',  ( 0.000000000000000000, 0.000000000000000000, 30.00000000000000000 ) ) ;
#18392 = VECTOR ( 'NONE', #10522, 1000.000000000000000 ) ;
#18393 = VERTEX_POINT ( 'NONE', #6550 ) ;
#18394 = ORIENTED_EDGE ( 'NONE', *, *, #10215, .T. ) ;
#18395 = VERTEX_POINT ( 'NONE', #17847 ) ;
#18396 = VECTOR ( 'NONE', #14404, 1000.000000000000000 ) ;
#18397 = EDGE_LOOP ( 'NONE', ( #4834, #5758, #6647, #6660 ) ) ;
#18398 = FACE_OUTER_BOUND ( 'NONE', #213, .T. ) ;
#18399 = CARTESIAN_POINT ( 'NONE',  ( -63.78533391645962780, -88.07278042982854060, 8.660254037844412167 ) ) ;
#18400 = ORIENTED_EDGE ( 'NONE', *, *, #14709, .F. ) ;
#18401 = CARTESIAN_POINT ( 'NONE',  ( -37.15834831208948685, -26.14378280364935137, 12.99038105676661736 ) ) ;
#18402 = AXIS2_PLACEMENT_3D ( 'NONE', #16507, #14624, #1821 ) ;
#18403 = DIRECTION ( 'NONE',  ( -0.1566598588826321192, 0.9876526153536342445, 7.798540720466731404E-17 ) ) ;
#18404 = DIRECTION ( 'NONE',  ( -0.9876526153536336894, -0.1566598588826349503, 0.000000000000000000 ) ) ;
#18405 =( NAMED_UNIT ( * ) SI_UNIT ( $, .STERADIAN. ) SOLID_ANGLE_UNIT ( ) );
#18406 = ADVANCED_FACE ( 'NONE', ( #10614 ), #16417, .F. ) ;
#18407 = ORIENTED_EDGE ( 'NONE', *, *, #13101, .T. ) ;
#18408 = EDGE_CURVE ( 'NONE', #11722, #6775, #11349, .T. ) ;
#18409 = EDGE_CURVE ( 'NONE', #4280, #2469, #14163, .T. ) ;
#18410 = CYLINDRICAL_SURFACE ( 'NONE', #2091, 1.500000000000000666 ) ;
#18411 = AXIS2_PLACEMENT_3D ( 'NONE', #1783, #7572, #374 ) ;
#18412 = ORIENTED_EDGE ( 'NONE', *, *, #11076, .F. ) ;
#18413 = DIRECTION ( 'NONE',  ( -0.1566598588826321747, 0.9876526153536343555, 0.000000000000000000 ) ) ;
#18414 = ORIENTED_EDGE ( 'NONE', *, *, #7985, .T. ) ;
#18415 = DIRECTION ( 'NONE',  ( 1.000000000000000000, 0.000000000000000000, -0.000000000000000000 ) ) ;
#18416 = VERTEX_POINT ( 'NONE', #12292 ) ;
#18417 = ORIENTED_EDGE ( 'NONE', *, *, #11211, .F. ) ;
#18418 = CARTESIAN_POINT ( 'NONE',  ( 0.000000000000000000, 0.000000000000000000, 20.00000000000000000 ) ) ;
#18419 = ADVANCED_FACE ( 'NONE', ( #9671 ), #8431, .F. ) ;
#18420 = DIRECTION ( 'NONE',  ( -0.9876526153536341335, -0.1566598588826327021, 0.000000000000000000 ) ) ;
#18422 = ORIENTED_EDGE ( 'NONE', *, *, #4677, .T. ) ;
#18421 = CYLINDRICAL_SURFACE ( 'NONE', #4799, 1.500000000000000888 ) ;
#18423 = CIRCLE ( 'NONE', #860, 171.3327290851023292 ) ;
#18424 = EDGE_LOOP ( 'NONE', ( #14121, #7552 ) ) ;
#18425 = AXIS2_PLACEMENT_3D ( 'NONE', #10132, #15839, #14230 ) ;
#18426 = CARTESIAN_POINT ( 'NONE',  ( -0.4108482230646762212, -15.25244508934120802, -21.65063509461098334 ) ) ;
#18427 = VERTEX_POINT ( 'NONE', #3956 ) ;
#18428 = ORIENTED_EDGE ( 'NONE', *, *, #16700, .F. ) ;
#18429 = AXIS2_PLACEMENT_3D ( 'NONE', #8877, #14739, #6031 ) ;
#18430 = CARTESIAN_POINT ( 'NONE',  ( -2.200000000000000178, 0.000000000000000000, 25.00000000000000000 ) ) ;
#18431 = CIRCLE ( 'NONE', #4139, 149.4844750268701148 ) ;
#18432 = EDGE_LOOP ( 'NONE', ( #6307, #2273, #379, #10589 ) ) ;
#18433 = DIRECTION ( 'NONE',  ( -0.1566598588826321192, 0.9876526153536342445, 7.798540720466731404E-17 ) ) ;
#18434 = CARTESIAN_POINT ( 'NONE',  ( -49.50400600400985951, -28.10203103968224170, -8.660254037844380193 ) ) ;
#18435 = AXIS2_PLACEMENT_3D ( 'NONE', #15132, #16666, #740 ) ;
#18436 = DIRECTION ( 'NONE',  ( -0.9876526153536336894, -0.1566598588826350336, 0.000000000000000000 ) ) ;
#18437 = DIRECTION ( 'NONE',  ( -0.1566598588826321192, 0.9876526153536342445, 7.798540720466730171E-17 ) ) ;
#18438 = CIRCLE ( 'NONE', #5675, 1.499999999999999556 ) ;
#18439 = CARTESIAN_POINT ( 'NONE',  ( -3.044698072211382112, -78.43819910854666944, 17.32050807568880657 ) ) ;
#18440 = ORIENTED_EDGE ( 'NONE', *, *, #8730, .T. ) ;
#18441 = DIRECTION ( 'NONE',  ( -0.1566598588826321192, 0.9876526153536342445, 7.798540720466731404E-17 ) ) ;
#18442 = DIRECTION ( 'NONE',  ( 0.000000000000000000, 0.000000000000000000, 1.000000000000000000 ) ) ;
#18443 = EDGE_CURVE ( 'NONE', #2583, #8675, #18139, .T. ) ;
#18444 = PRODUCT_DEFINITION_FORMATION_WITH_SPECIFIED_SOURCE ( 'ANY', '', #454, .NOT_KNOWN. ) ;
#18445 = AXIS2_PLACEMENT_3D ( 'NONE', #6777, #11097, #3887 ) ;
#18446 = DIRECTION ( 'NONE',  ( 1.000000000000000000, 0.000000000000000000, 0.000000000000000000 ) ) ;
#18447 = EDGE_LOOP ( 'NONE', ( #14319, #185, #18149, #1890 ) ) ;
#18448 = EDGE_CURVE ( 'NONE', #7294, #14450, #14464, .T. ) ;
#18449 = ORIENTED_EDGE ( 'NONE', *, *, #17291, .F. ) ;
#18450 = DIRECTION ( 'NONE',  ( -0.9876526153536336894, -0.1566598588826349503, 0.000000000000000000 ) ) ;
#18451 = CIRCLE ( 'NONE', #8397, 1.500000000000000888 ) ;
#18452 = FACE_BOUND ( 'NONE', #16072, .T. ) ;
#18453 = AXIS2_PLACEMENT_3D ( 'NONE', #2720, #2533, #7106 ) ;
#18454 = AXIS2_PLACEMENT_3D ( 'NONE', #16985, #15537, #9848 ) ;
#18455 = ORIENTED_EDGE ( 'NONE', *, *, #2607, .F. ) ;
#18456 = ORIENTED_EDGE ( 'NONE', *, *, #543, .F. ) ;
#18457 = DIRECTION ( 'NONE',  ( -0.1566598588826321192, 0.9876526153536342445, 7.798540720466730171E-17 ) ) ;
#18458 = AXIS2_PLACEMENT_3D ( 'NONE', #14858, #7674, #2061 ) ;
#18459 = CARTESIAN_POINT ( 'NONE',  ( -73.49714175923330117, -26.84527464665595886, 1.908195823574487804E-14 ) ) ;
#18460 = CARTESIAN_POINT ( 'NONE',  ( -37.94164760650263446, -21.20551972688122078, 4.330127018922218518 ) ) ;
#18461 = CARTESIAN_POINT ( 'NONE',  ( 2.000000000000000000, 0.000000000000000000, -25.65685424949237614 ) ) ;
#18462 = EDGE_CURVE ( 'NONE', #3287, #6534, #15977, .T. ) ;
#18463 = CIRCLE ( 'NONE', #16918, 1.500000000000000888 ) ;
#18464 = CIRCLE ( 'NONE', #13897, 1.500000000000000444 ) ;
#18465 = CARTESIAN_POINT ( 'NONE',  ( -3.000000000000004441, 0.000000000000000000, -22.00000000000000711 ) ) ;
#18466 = EDGE_CURVE ( 'NONE', #13075, #11927, #8716, .T. ) ;
#18467 = MECHANICAL_DESIGN_GEOMETRIC_PRESENTATION_REPRESENTATION (  '', ( #12022 ), #6939 ) ;
#18468 = EDGE_CURVE ( 'NONE', #12073, #2, #240, .T. ) ;
#18469 = CARTESIAN_POINT ( 'NONE',  ( -35.67686938905902849, -25.90879301532540779, 21.65063509461101887 ) ) ;
#18470 = EDGE_LOOP ( 'NONE', ( #18260, #7290 ) ) ;
#18471 = ORIENTED_EDGE ( 'NONE', *, *, #9439, .T. ) ;
#18472 = CARTESIAN_POINT ( 'NONE',  ( 73.09088021254186174, 1.387778780781445676E-14, -19.99999999999999645 ) ) ;
#18473 = ORIENTED_EDGE ( 'NONE', *, *, #12171, .F. ) ;
#18474 = ORIENTED_EDGE ( 'NONE', *, *, #13328, .F. ) ;
#18475 = CARTESIAN_POINT ( 'NONE',  ( -60.32854976272193426, -87.52447092373932946, -8.660254037844385522 ) ) ;
#18476 = VECTOR ( 'NONE', #13295, 1000.000000000000000 ) ;
#18477 = CIRCLE ( 'NONE', #16932, 1.500000000000000888 ) ;
#18478 = VECTOR ( 'NONE', #3703, 1000.000000000000000 ) ;
#18479 = CARTESIAN_POINT ( 'NONE',  ( -351.9873556332902922, 23.03471749664299395, 2.567204941047428095E-15 ) ) ;
#18480 = ITEM_DEFINED_TRANSFORMATION ( 'NONE', 'NONE', #7208,  #18772 ) ;
#18481 = DIRECTION ( 'NONE',  ( -0.1566598588826321747, 0.9876526153536343555, 0.000000000000000000 ) ) ;
#18482 = CARTESIAN_POINT ( 'NONE',  ( 1.399738696879940791, -77.73322974357483872, 21.65063509461100821 ) ) ;
#18483 = EDGE_LOOP ( 'NONE', ( #12432, #8578 ) ) ;
#18484 = EDGE_CURVE ( 'NONE', #5191, #10544, #11587, .T. ) ;
#18485 = CARTESIAN_POINT ( 'NONE',  ( -24.11451099155181055, -19.01228170252437266, -8.660254037844380193 ) ) ;
#18486 = DIRECTION ( 'NONE',  ( -0.1566598588826321192, 0.9876526153536342445, 7.798540720466730171E-17 ) ) ;
#18487 = ADVANCED_FACE ( 'NONE', ( #14208 ), #970, .F. ) ;
#18488 = ORIENTED_EDGE ( 'NONE', *, *, #4266, .F. ) ;
#18489 = EDGE_LOOP ( 'NONE', ( #17023, #7779, #3265, #124 ) ) ;
#18490 = DIRECTION ( 'NONE',  ( 0.000000000000000000, 0.000000000000000000, 1.000000000000000000 ) ) ;
#18491 = CYLINDRICAL_SURFACE ( 'NONE', #13947, 1.500000000000001554 ) ;
#18492 = CIRCLE ( 'NONE', #7842, 1.500000000000000444 ) ;
#18493 = EDGE_LOOP ( 'NONE', ( #10677, #16836, #1376, #15863 ) ) ;
#18494 = VECTOR ( 'NONE', #7747, 1000.000000000000000 ) ;
#18495 = CARTESIAN_POINT ( 'NONE',  ( -309.0881213225398483, -2.850701963179328668, 9.951701414186818625E-16 ) ) ;
#18496 = AXIS2_PLACEMENT_3D ( 'NONE', #11563, #5718, #10241 ) ;
#18497 = ORIENTED_EDGE ( 'NONE', *, *, #242, .F. ) ;
#18498 = ORIENTED_EDGE ( 'NONE', *, *, #708, .F. ) ;
#18499 = CARTESIAN_POINT ( 'NONE',  ( -25.80034323552273179, -24.34219442649909126, -21.65063509461098334 ) ) ;
#18500 = ORIENTED_EDGE ( 'NONE', *, *, #17349, .T. ) ;
#18501 = DIRECTION ( 'NONE',  ( -0.1566598588826321192, 0.9876526153536342445, 7.798540720466730171E-17 ) ) ;
#18502 = ORIENTED_EDGE ( 'NONE', *, *, #13085, .F. ) ;
#18503 = CIRCLE ( 'NONE', #271, 1.500000000000000888 ) ;
#18504 = DIRECTION ( 'NONE',  ( 0.000000000000000000, 0.000000000000000000, 1.000000000000000000 ) ) ;
#18505 = DIRECTION ( 'NONE',  ( -0.1566598588826321192, 0.9876526153536342445, 7.798540720466730171E-17 ) ) ;
#18506 = AXIS2_PLACEMENT_3D ( 'NONE', #3865, #9684, #15459 ) ;
#18507 = CARTESIAN_POINT ( 'NONE',  ( -32.22008523532133495, -25.36048350923618955, -21.65063509461098334 ) ) ;
#18508 =( LENGTH_UNIT ( ) NAMED_UNIT ( * ) SI_UNIT ( .MILLI., .METRE. ) );
#18509 = AXIS2_PLACEMENT_3D ( 'NONE', #2960, #10078, #17493 ) ;
#18510 = CARTESIAN_POINT ( 'NONE',  ( -5.349111299832828514, -16.03574438375436984, -21.65063509461098334 ) ) ;
#18511 = AXIS2_PLACEMENT_3D ( 'NONE', #4957, #14591, #8978 ) ;
#18512 = VERTEX_POINT ( 'NONE', #13812 ) ;
#18513 = DIRECTION ( 'NONE',  ( -0.9876526153536336894, -0.1566598588826349503, 0.000000000000000000 ) ) ;
#18514 = CARTESIAN_POINT ( 'NONE',  ( 0.000000000000000000, 0.000000000000000000, 37.00000000000000711 ) ) ;
#18515 = VERTEX_POINT ( 'NONE', #5215 ) ;
#18516 = DIRECTION ( 'NONE',  ( -0.1566598588826321192, 0.9876526153536342445, 7.798540720466731404E-17 ) ) ;
#18517 = DIRECTION ( 'NONE',  ( 0.000000000000000000, 0.000000000000000000, 1.000000000000000000 ) ) ;
#18518 = EDGE_LOOP ( 'NONE', ( #549, #17069, #9837, #14681 ) ) ;
#18519 = VECTOR ( 'NONE', #1483, 1000.000000000000000 ) ;
#18520 = DIRECTION ( 'NONE',  ( -1.000000000000000000, 0.000000000000000000, 0.000000000000000000 ) ) ;
#18521 = EDGE_LOOP ( 'NONE', ( #1482, #8303 ) ) ;
#18522 = EDGE_LOOP ( 'NONE', ( #4318, #146 ) ) ;
#18523 = EDGE_CURVE ( 'NONE', #6427, #15929, #17079, .T. ) ;
#18524 = CIRCLE ( 'NONE', #11181, 1.499999999999999556 ) ;
#18525 = EDGE_CURVE ( 'NONE', #3315, #1682, #9924, .T. ) ;
#18526 = CARTESIAN_POINT ( 'NONE',  ( -71.23236354178969520, -31.54854793510013877, 1.887572821959364500E-14 ) ) ;
#18527 = CARTESIAN_POINT ( 'NONE',  ( 3.000000000000000000, 0.000000000000000000, 30.00000000000000000 ) ) ;
#18528 = EDGE_CURVE ( 'NONE', #8040, #3775, #8420, .T. ) ;
#18529 = CARTESIAN_POINT ( 'NONE',  ( 0.000000000000000000, 0.000000000000000000, -37.00000000000000711 ) ) ;
#18530 = CARTESIAN_POINT ( 'NONE',  ( -11.93357161039406300, -79.84813783849035929, -12.99038105676658539 ) ) ;
#18531 = CARTESIAN_POINT ( 'NONE',  ( -75.96627329761737712, -27.23692429386253622, -4.330127018922180326 ) ) ;
#18532 = AXIS2_PLACEMENT_3D ( 'NONE', #11696, #15896, #14477 ) ;
#18533 = CYLINDRICAL_SURFACE ( 'NONE', #17854, 1.500000000000001554 ) ;
#18534 = DIRECTION ( 'NONE',  ( 1.000000000000000000, 0.000000000000000000, 0.000000000000000000 ) ) ;
#18535 = FACE_BOUND ( 'NONE', #9919, .T. ) ;
#18536 = CARTESIAN_POINT ( 'NONE',  ( -62.00000000000000000, 0.000000000000000000, -25.00000000000000000 ) ) ;
#18537 = CARTESIAN_POINT ( 'NONE',  ( -56.37793930130741415, -86.89783148820879433, -12.99038105676658539 ) ) ;
#18538 = CIRCLE ( 'NONE', #12094, 1.500000000000000888 ) ;
#18539 = ORIENTED_EDGE ( 'NONE', *, *, #2080, .F. ) ;
#18540 = CIRCLE ( 'NONE', #8204, 1.499999999999999556 ) ;
#18541 = EDGE_LOOP ( 'NONE', ( #6957, #18313, #11816, #203 ) ) ;
#18542 = DIRECTION ( 'NONE',  ( -0.9876526153536341335, -0.1566598588826327021, 0.000000000000000000 ) ) ;
#18543 = PRODUCT ( 'Upper Squeezer Handle Arm', 'Upper Squeezer Handle Arm', '', ( #18667 ) ) ;
#18544 = ORIENTED_EDGE ( 'NONE', *, *, #1119, .F. ) ;
#18545 = ORIENTED_EDGE ( 'NONE', *, *, #17436, .T. ) ;
#18546 = CIRCLE ( 'NONE', #11801, 1.500000000000000888 ) ;
#18547 = DIRECTION ( 'NONE',  ( 0.000000000000000000, 0.000000000000000000, 1.000000000000000000 ) ) ;
#18548 = CIRCLE ( 'NONE', #10001, 1.500000000000000888 ) ;
#18549 = DIRECTION ( 'NONE',  ( -0.1566598588826321192, 0.9876526153536342445, 7.798540720466731404E-17 ) ) ;
#18550 = ADVANCED_FACE ( 'NONE', ( #2641 ), #1156, .F. ) ;
#18551 = CYLINDRICAL_SURFACE ( 'NONE', #6456, 1.500000000000001554 ) ;
#18552 = ORIENTED_EDGE ( 'NONE', *, *, #14304, .T. ) ;
#18553 = CIRCLE ( 'NONE', #15773, 1.500000000000000888 ) ;
#18554 = LINE ( 'NONE', #14132, #9663 ) ;
#18555 = DIRECTION ( 'NONE',  ( 0.1856185419698762329, -0.9826218788918640312, 0.000000000000000000 ) ) ;
#18556 = EDGE_LOOP ( 'NONE', ( #11336, #12974, #15043, #3763 ) ) ;
#18557 = EDGE_CURVE ( 'NONE', #13791, #6631, #16594, .T. ) ;
#18558 = AXIS2_PLACEMENT_3D ( 'NONE', #2405, #10819, #17901 ) ;
#18559 = CARTESIAN_POINT ( 'NONE',  ( -51.97313754239392125, -28.49368068688881550, 21.65063509461101887 ) ) ;
#18560 = CARTESIAN_POINT ( 'NONE',  ( -39.09401853261890381, -84.15628395776272441, -17.32050807568878525 ) ) ;
#18561 = CARTESIAN_POINT ( 'NONE',  ( -94.14047854185179176, 6.938893903907228378E-15, 2.500000000000000000 ) ) ;
#18562 = EDGE_LOOP ( 'NONE', ( #5956, #17133, #8418, #3288 ) ) ;
#18563 = DIRECTION ( 'NONE',  ( -0.9876526153536336894, -0.1566598588826349503, 0.000000000000000000 ) ) ;
#18564 = AXIS2_PLACEMENT_3D ( 'NONE', #2743, #8536, #11343 ) ;
#18565 = ORIENTED_EDGE ( 'NONE', *, *, #13149, .F. ) ;
#18566 = ORIENTED_EDGE ( 'NONE', *, *, #5486, .F. ) ;
#18567 = AXIS2_PLACEMENT_3D ( 'NONE', #15382, #15202, #7996 ) ;
#18568 = ORIENTED_EDGE ( 'NONE', *, *, #16916, .F. ) ;
#18569 = ORIENTED_EDGE ( 'NONE', *, *, #18707, .T. ) ;
#18570 = DIRECTION ( 'NONE',  ( 0.000000000000000000, -1.445602896647338917E-16, 1.000000000000000000 ) ) ;
#18571 = ORIENTED_EDGE ( 'NONE', *, *, #8209, .T. ) ;
#18572 = ORIENTED_EDGE ( 'NONE', *, *, #15950, .F. ) ;
#18573 = CARTESIAN_POINT ( 'NONE',  ( -129.1237108893556638, -14.52091123662038896, 5.132104245558540612 ) ) ;
#18574 = CIRCLE ( 'NONE', #16719, 2.200000000000000178 ) ;
#18575 = CARTESIAN_POINT ( 'NONE',  ( -70.00000000000000000, 44.99999999999999289, -25.00000000000000000 ) ) ;
#18576 = EDGE_CURVE ( 'NONE', #9820, #17569, #12670, .T. ) ;
#18577 = AXIS2_PLACEMENT_3D ( 'NONE', #5214, #14016, #1248 ) ;
#18578 = UNCERTAINTY_MEASURE_WITH_UNIT (LENGTH_MEASURE( 1.000000000000000082E-05 ), #10098, 'distance_accuracy_value', 'NONE');
#18579 = CARTESIAN_POINT ( 'NONE',  ( -75.18297400320422241, -32.17518737063066681, -21.65063509461098334 ) ) ;
#18580 = LINE ( 'NONE', #14353, #883 ) ;
#18581 = EDGE_CURVE ( 'NONE', #2601, #15004, #4172, .T. ) ;
#18582 = AXIS2_PLACEMENT_3D ( 'NONE', #7589, #6263, #11995 ) ;
#18583 = ORIENTED_EDGE ( 'NONE', *, *, #14732, .T. ) ;
#18584 = CYLINDRICAL_SURFACE ( 'NONE', #15735, 1.500000000000001554 ) ;
#18585 = CARTESIAN_POINT ( 'NONE',  ( -21.81009776393036503, -81.41473642731669713, 21.65063509461101532 ) ) ;
#18586 = ORIENTED_EDGE ( 'NONE', *, *, #5344, .T. ) ;
#18587 = COLOUR_RGB ( '', 0.31764706, 0.68627451, 0.89019608) ;
#18588 = CARTESIAN_POINT ( 'NONE',  ( -13.25033222266188560, -17.28902325481542235, 12.99038105676661381 ) ) ;
#18589 = ORIENTED_EDGE ( 'NONE', *, *, #10987, .T. ) ;
#18590 = VERTEX_POINT ( 'NONE', #9931 ) ;
#18591 = CARTESIAN_POINT ( 'NONE',  ( 1.360103686702108128, -20.03404830722672259, 17.32050807568881012 ) ) ;
#18592 = FACE_OUTER_BOUND ( 'NONE', #18397, .T. ) ;
#18593 = CIRCLE ( 'NONE', #686, 1.500000000000000888 ) ;
#18594 = CARTESIAN_POINT ( 'NONE',  ( 0.000000000000000000, 0.000000000000000000, 32.00000000000000000 ) ) ;
#18595 = ADVANCED_FACE ( 'NONE', ( #13056, #14314 ), #10031, .F. ) ;
#18596 = VERTEX_POINT ( 'NONE', #173 ) ;
#18597 = CARTESIAN_POINT ( 'NONE',  ( -51.43967622453926936, -86.11453219379562540, -12.99038105676658539 ) ) ;
#18598 = ADVANCED_FACE ( 'NONE', ( #15904 ), #2744, .F. ) ;
#18599 = CARTESIAN_POINT ( 'NONE',  ( -70.00000000000000000, 44.99999999999999289, 25.00000000000000000 ) ) ;
#18600 = EDGE_CURVE ( 'NONE', #11742, #9953, #1518, .T. ) ;
#18601 = EDGE_CURVE ( 'NONE', #10401, #5894, #237, .T. ) ;
#18602 = DIRECTION ( 'NONE',  ( -0.1566598588826321192, 0.9876526153536342445, 7.798540720466730171E-17 ) ) ;
#18603 = EDGE_CURVE ( 'NONE', #5396, #13454, #4428, .T. ) ;
#18604 = CYLINDRICAL_SURFACE ( 'NONE', #10628, 1.500000000000001554 ) ;
#18605 = CARTESIAN_POINT ( 'NONE',  ( -42.09661138885763165, -26.92708209806250608, 4.330127018922217630 ) ) ;
#18606 = CARTESIAN_POINT ( 'NONE',  ( -27.57129514528951120, -19.56059120861358736, -8.660254037844380193 ) ) ;
#18607 =( LENGTH_UNIT ( ) NAMED_UNIT ( * ) SI_UNIT ( .MILLI., .METRE. ) );
#18608 = AXIS2_PLACEMENT_3D ( 'NONE', #412, #18055, #12025 ) ;
#18609 = CYLINDRICAL_SURFACE ( 'NONE', #3877, 1.500000000000001554 ) ;
#18610 = ORIENTED_EDGE ( 'NONE', *, *, #2667, .F. ) ;
#18611 = DIRECTION ( 'NONE',  ( -0.1566598588826321747, 0.9876526153536343555, 0.000000000000000000 ) ) ;
#18612 = CARTESIAN_POINT ( 'NONE',  ( -41.39843176024032800, -21.75382923297043192, 4.330127018922218518 ) ) ;
#18613 = DIRECTION ( 'NONE',  ( -1.000000000000000000, 0.000000000000000000, 0.000000000000000000 ) ) ;
#18614 = ORIENTED_EDGE ( 'NONE', *, *, #12195, .T. ) ;
#18615 = DIRECTION ( 'NONE',  ( -0.1566598588826321192, 0.9876526153536342445, 7.798540720466731404E-17 ) ) ;
#18616 = CARTESIAN_POINT ( 'NONE',  ( -79.05438463828195950, 1.499069270643396345, 3.389939594122236333 ) ) ;
#18617 = ORIENTED_EDGE ( 'NONE', *, *, #10015, .F. ) ;
#18618 = ORIENTED_EDGE ( 'NONE', *, *, #13364, .F. ) ;
#18619 = VERTEX_POINT ( 'NONE', #8537 ) ;
#18620 = VERTEX_POINT ( 'NONE', #14488 ) ;
#18621 = CIRCLE ( 'NONE', #7665, 1.500000000000000888 ) ;
#18622 = DIRECTION ( 'NONE',  ( 0.000000000000000000, 0.000000000000000000, 1.000000000000000000 ) ) ;
#18623 = ORIENTED_EDGE ( 'NONE', *, *, #11715, .T. ) ;
#18624 = CARTESIAN_POINT ( 'NONE',  ( -11.76885329963143079, -17.05403346649147878, 12.99038105676661381 ) ) ;
#18625 = CARTESIAN_POINT ( 'NONE',  ( -50.28730529842301422, -23.16376796291411111, -8.660254037844380193 ) ) ;
#18626 = DIRECTION ( 'NONE',  ( -0.9876526153536336894, -0.1566598588826349503, 0.000000000000000000 ) ) ;
#18627 = DIRECTION ( 'NONE',  ( -0.9876526153536336894, -0.1566598588826349503, 0.000000000000000000 ) ) ;
#18628 = DIRECTION ( 'NONE',  ( -0.1566598588826321747, 0.9876526153536343555, 0.000000000000000000 ) ) ;
#18629 = CYLINDRICAL_SURFACE ( 'NONE', #17942, 1.500000000000001554 ) ;
#18630 = CARTESIAN_POINT ( 'NONE',  ( -39.91695283720989096, -21.51883944464648124, -12.99038105676658006 ) ) ;
#18631 = FACE_BOUND ( 'NONE', #1167, .T. ) ;
#18632 = ADVANCED_FACE ( 'NONE', ( #4526 ), #5874, .F. ) ;
#18633 = EDGE_CURVE ( 'NONE', #17212, #9621, #6924, .T. ) ;
#18634 = DIRECTION ( 'NONE',  ( -0.1566598588826321192, 0.9876526153536342445, 7.798540720466730171E-17 ) ) ;
#18635 = AXIS2_PLACEMENT_3D ( 'NONE', #7120, #88, #10204 ) ;
#18637 = ORIENTED_EDGE ( 'NONE', *, *, #13971, .F. ) ;
#18636 = DIRECTION ( 'NONE',  ( 0.000000000000000000, 0.000000000000000000, 1.000000000000000000 ) ) ;
#18638 = ORIENTED_EDGE ( 'NONE', *, *, #8154, .T. ) ;
#18639 = CARTESIAN_POINT ( 'NONE',  ( -47.32434745236211171, -22.69378838626622041, -8.660254037844380193 ) ) ;
#18640 = ORIENTED_EDGE ( 'NONE', *, *, #4028, .T. ) ;
#18641 = ORIENTED_EDGE ( 'NONE', *, *, #16184, .F. ) ;
#18642 = CARTESIAN_POINT ( 'NONE',  ( 1.360103686702108128, -20.03404830722672259, -17.32050807568878170 ) ) ;
#18643 = EDGE_LOOP ( 'NONE', ( #12492, #4752, #9342, #10402, #7152, #7006, #1713, #1073, #14657, #14707, #11382, #1635 ) ) ;
#18644 = CARTESIAN_POINT ( 'NONE',  ( -6.047290928450125946, -21.20899724884646531, 12.99038105676661026 ) ) ;
#18645 = DIRECTION ( 'NONE',  ( -0.1566598588826321192, 0.9876526153536342445, 7.798540720466731404E-17 ) ) ;
#18646 = EDGE_LOOP ( 'NONE', ( #16757, #16505, #4188, #13872 ) ) ;
#18647 = CYLINDRICAL_SURFACE ( 'NONE', #1772, 20.00000000000001066 ) ;
#18648 = FACE_BOUND ( 'NONE', #9947, .T. ) ;
#18649 = ADVANCED_FACE ( 'NONE', ( #14400 ), #17163, .F. ) ;
#18650 = LINE ( 'NONE', #11186, #6854 ) ;
#18651 = CARTESIAN_POINT ( 'NONE',  ( -77.40662104346073136, 32.93835651487657401, 35.00000000000000000 ) ) ;
#18652 = CARTESIAN_POINT ( 'NONE',  ( -63.78533391645962780, -88.07278042982852639, -8.660254037844385522 ) ) ;
#18653 = DIRECTION ( 'NONE',  ( -0.9826218788918640312, -0.1856185419698769823, 0.000000000000000000 ) ) ;
#18654 = CYLINDRICAL_SURFACE ( 'NONE', #5733, 2.000000000000000000 ) ;
#18655 = EDGE_CURVE ( 'NONE', #14342, #5230, #3011, .T. ) ;
#18656 = ORIENTED_EDGE ( 'NONE', *, *, #3962, .F. ) ;
#18657 = ORIENTED_EDGE ( 'NONE', *, *, #3170, .F. ) ;
#18658 = ORIENTED_EDGE ( 'NONE', *, *, #6746, .T. ) ;
#18659 = DIRECTION ( 'NONE',  ( 0.000000000000000000, 0.000000000000000000, 1.000000000000000000 ) ) ;
#18660 = EDGE_LOOP ( 'NONE', ( #402, #10322, #6122, #10713 ) ) ;
#18661 = ORIENTED_EDGE ( 'NONE', *, *, #14159, .T. ) ;
#18662 = CIRCLE ( 'NONE', #17112, 1.500000000000000888 ) ;
#18663 = FACE_BOUND ( 'NONE', #13908, .T. ) ;
#18664 = CARTESIAN_POINT ( 'NONE',  ( -170.5980861165185445, 32.53234180668174247, 5.500000000000001776 ) ) ;
#18665 = CARTESIAN_POINT ( 'NONE',  ( -56.21322099054479082, -24.10372711620989961, -12.99038105676658006 ) ) ;
#18666 = FACE_OUTER_BOUND ( 'NONE', #8441, .T. ) ;
#18667 = PRODUCT_CONTEXT ( 'NONE', #5926, 'mechanical' ) ;
#18668 = EDGE_LOOP ( 'NONE', ( #14251, #12816 ) ) ;
#18669 = CARTESIAN_POINT ( 'NONE',  ( -16.70711637639958269, -17.83733276090463349, -21.65063509461097979 ) ) ;
#18670 = CARTESIAN_POINT ( 'NONE',  ( -6.830590222863280658, -16.27073417207831696, 4.330127018922214965 ) ) ;
#18671 = CARTESIAN_POINT ( 'NONE',  ( -56.91140061916209447, -29.27697998130198442, -4.330127018922181215 ) ) ;
#18672 = CARTESIAN_POINT ( 'NONE',  ( -30.20514499443621759, -82.74634522781903456, -21.65063509461098690 ) ) ;
#18673 = VERTEX_POINT ( 'NONE', #12956 ) ;
#18674 = EDGE_LOOP ( 'NONE', ( #7617, #14931 ) ) ;
#18675 = LINE ( 'NONE', #12737, #16664 ) ;
#18676 = FACE_OUTER_BOUND ( 'NONE', #5679, .T. ) ;
#18677 = ADVANCED_FACE ( 'NONE', ( #11531 ), #8799, .F. ) ;
#18678 = DIRECTION ( 'NONE',  ( -0.1566598588826321192, 0.9876526153536342445, 7.798540720466730171E-17 ) ) ;
#18679 = ORIENTED_EDGE ( 'NONE', *, *, #7689, .T. ) ;
#18680 = DIRECTION ( 'NONE',  ( -0.1566598588826321192, 0.9876526153536342445, 7.798540720466730171E-17 ) ) ;
#18681 = EDGE_CURVE ( 'NONE', #6631, #14196, #18714, .T. ) ;
#18682 = EDGE_LOOP ( 'NONE', ( #1951, #2396 ) ) ;
#18683 = AXIS2_PLACEMENT_3D ( 'NONE', #11586, #17408, #5643 ) ;
#18684 = DIRECTION ( 'NONE',  ( 0.9868632313631133801, 0.1615579233078773547, -0.000000000000000000 ) ) ;
#18685 = EDGE_LOOP ( 'NONE', ( #18065, #10890 ) ) ;
#18686 = LINE ( 'NONE', #11408, #7604 ) ;
#18687 = DIRECTION ( 'NONE',  ( -0.1566598588826321192, 0.9876526153536342445, 7.798540720466731404E-17 ) ) ;
#18688 = CARTESIAN_POINT ( 'NONE',  ( -55.42992169613161479, -29.04199019297804085, 21.65063509461101887 ) ) ;
#18689 = SURFACE_SIDE_STYLE ('',( #7103 ) ) ;
#18690 = EDGE_LOOP ( 'NONE', ( #10195, #9290 ) ) ;
#18691 = CIRCLE ( 'NONE', #11943, 1.500000000000000888 ) ;
#18692 = FACE_OUTER_BOUND ( 'NONE', #13805, .T. ) ;
#18693 = ORIENTED_EDGE ( 'NONE', *, *, #4150, .F. ) ;
#18694 = CARTESIAN_POINT ( 'NONE',  ( -52.92115514756972061, -86.34952198211958319, -21.65063509461098690 ) ) ;
#18695 = CARTESIAN_POINT ( 'NONE',  ( -79.05438463828195950, 1.499069270643396345, 3.389939594122236333 ) ) ;
#18696 = CARTESIAN_POINT ( 'NONE',  ( -57.89905323451570496, -29.43363984018461466, 17.32050807568881723 ) ) ;
#18697 = CYLINDRICAL_SURFACE ( 'NONE', #7592, 1.500000000000001554 ) ;
#18698 = AXIS2_PLACEMENT_3D ( 'NONE', #16109, #3104, #8896 ) ;
#18700 = ORIENTED_EDGE ( 'NONE', *, *, #12138, .F. ) ;
#18699 = DIRECTION ( 'NONE',  ( -0.1566598588826321192, 0.9876526153536342445, 7.798540720466730171E-17 ) ) ;
#18701 = EDGE_CURVE ( 'NONE', #3501, #4575, #11131, .T. ) ;
#18702 = ADVANCED_FACE ( 'NONE', ( #17543 ), #10307, .F. ) ;
#18703 = CARTESIAN_POINT ( 'NONE',  ( -84.16561914167408531, 33.59999999999999432, -24.99999999999999289 ) ) ;
#18704 = DIRECTION ( 'NONE',  ( -0.1566598588826321192, 0.9876526153536342445, 7.798540720466731404E-17 ) ) ;
#18705 = VERTEX_POINT ( 'NONE', #11434 ) ;
#18706 = VERTEX_POINT ( 'NONE', #17273 ) ;
#18707 = EDGE_CURVE ( 'NONE', #9998, #11894, #12340, .T. ) ;
#18708 = AXIS2_PLACEMENT_3D ( 'NONE', #13452, #6289, #303 ) ;
#18709 = FACE_OUTER_BOUND ( 'NONE', #16286, .T. ) ;
#18710 = ORIENTED_EDGE ( 'NONE', *, *, #16353, .T. ) ;
#18711 = CARTESIAN_POINT ( 'NONE',  ( -11.93357161039406300, -79.84813783849037350, 12.99038105676661203 ) ) ;
#18712 = VECTOR ( 'NONE', #17060, 1000.000000000000000 ) ;
#18713 = CARTESIAN_POINT ( 'NONE',  ( -4.526176995241833367, -78.67318889687062722, 1.424741226644455312E-14 ) ) ;
#18714 = LINE ( 'NONE', #8707, #9937 ) ;
#18715 = CARTESIAN_POINT ( 'NONE',  ( -0.5755665338273054932, -78.04654946134009208, 21.65063509461100821 ) ) ;
#18716 = DIRECTION ( 'NONE',  ( 0.000000000000000000, 0.000000000000000000, 1.000000000000000000 ) ) ;
#18717 = CARTESIAN_POINT ( 'NONE',  ( -16.87183468716221313, -80.63143713290352821, -21.65063509461098690 ) ) ;
#18718 = CARTESIAN_POINT ( 'NONE',  ( -15.22563745336913144, -17.60234297258068992, -12.99038105676658006 ) ) ;
#18719 = ORIENTED_EDGE ( 'NONE', *, *, #5083, .T. ) ;
#18721 = ORIENTED_EDGE ( 'NONE', *, *, #3350, .F. ) ;
#18720 = EDGE_CURVE ( 'NONE', #10673, #6102, #2375, .T. ) ;
#18722 = DIRECTION ( 'NONE',  ( -0.1566598588826321192, 0.9876526153536342445, 7.798540720466730171E-17 ) ) ;
#18723 = AXIS2_PLACEMENT_3D ( 'NONE', #10375, #17802, #7825 ) ;
#18724 = ORIENTED_EDGE ( 'NONE', *, *, #11185, .F. ) ;
#18725 = ORIENTED_EDGE ( 'NONE', *, *, #9241, .F. ) ;
#18726 = DIRECTION ( 'NONE',  ( -0.9876526153536341335, -0.1566598588826327021, 0.000000000000000000 ) ) ;
#18727 = CIRCLE ( 'NONE', #1440, 1.499999999999999556 ) ;
#18728 = DIRECTION ( 'NONE',  ( 0.1566598588826321192, -0.9876526153536342445, -7.798540720466731404E-17 ) ) ;
#18729 = AXIS2_PLACEMENT_3D ( 'NONE', #1134, #1232, #1052 ) ;
#18730 = CIRCLE ( 'NONE', #13814, 1.500000000000000888 ) ;
#18731 = ORIENTED_EDGE ( 'NONE', *, *, #16669, .F. ) ;
#18732 = AXIS2_PLACEMENT_3D ( 'NONE', #9890, #10079, #5641 ) ;
#18733 =( GEOMETRIC_REPRESENTATION_CONTEXT ( 3 ) GLOBAL_UNCERTAINTY_ASSIGNED_CONTEXT ( ( #17032 ) ) GLOBAL_UNIT_ASSIGNED_CONTEXT ( ( #16173, #3253, #7542 ) ) REPRESENTATION_CONTEXT ( 'NONE', 'WORKASPACE' ) );
#18734 = CIRCLE ( 'NONE', #13506, 1.500000000000000888 ) ;
#18735 = CYLINDRICAL_SURFACE ( 'NONE', #16063, 1.500000000000001554 ) ;
#18736 = DIRECTION ( 'NONE',  ( -0.1566598588826321747, 0.9876526153536343555, 0.000000000000000000 ) ) ;
#18737 = DIRECTION ( 'NONE',  ( 0.000000000000000000, 0.000000000000000000, 1.000000000000000000 ) ) ;
#18738 = CIRCLE ( 'NONE', #10208, 1.500000000000000888 ) ;
#18739 = CARTESIAN_POINT ( 'NONE',  ( -63.78533391645962780, -88.07278042982852639, 1.424741226644455312E-14 ) ) ;
#18740 = ORIENTED_EDGE ( 'NONE', *, *, #1830, .F. ) ;
#18741 = ORIENTED_EDGE ( 'NONE', *, *, #12741, .F. ) ;
#18742 = ORIENTED_EDGE ( 'NONE', *, *, #11156, .F. ) ;
#18743 = ORIENTED_EDGE ( 'NONE', *, *, #2404, .F. ) ;
#18744 = CARTESIAN_POINT ( 'NONE',  ( -77.18258565727082043, 4.450738551673809162, -20.00000000000001776 ) ) ;
#18745 = EDGE_LOOP ( 'NONE', ( #8541, #8448, #17738, #18182 ) ) ;
#18746 = PRODUCT_DEFINITION_FORMATION_WITH_SPECIFIED_SOURCE ( 'ANY', '', #9076, .NOT_KNOWN. ) ;
#18747 = PLANE ( 'NONE',  #9137 ) ;
#18748 = ADVANCED_FACE ( 'NONE', ( #7670 ), #1962, .F. ) ;
#18749 = AXIS2_PLACEMENT_3D ( 'NONE', #144, #18678, #17503 ) ;
#18750 = CARTESIAN_POINT ( 'NONE',  ( -33.20773785067495965, -25.51714336811882688, 17.32050807568881723 ) ) ;
#18751 = EDGE_CURVE ( 'NONE', #11320, #5805, #13865, .T. ) ;
#18752 = ADVANCED_FACE ( 'NONE', ( #6057 ), #14780, .T. ) ;
#18753 = AXIS2_PLACEMENT_3D ( 'NONE', #12274, #17932, #4898 ) ;
#18754 = DIRECTION ( 'NONE',  ( 0.000000000000000000, 0.000000000000000000, 1.000000000000000000 ) ) ;
#18755 = SHAPE_DEFINITION_REPRESENTATION ( #10586, #5397 ) ;
#18756 = AXIS2_PLACEMENT_3D ( 'NONE', #723, #17620, #630 ) ;
#18757 = CARTESIAN_POINT ( 'NONE',  ( -0.4108482230646692823, -15.25244508934120802, 4.330127018922213189 ) ) ;
#18758 = CARTESIAN_POINT ( 'NONE',  ( -81.73462711737164454, 33.01666666666666572, 25.00000000000001421 ) ) ;
#18759 = DIRECTION ( 'NONE',  ( 0.000000000000000000, 0.000000000000000000, 1.000000000000000000 ) ) ;
#18760 = AXIS2_PLACEMENT_3D ( 'NONE', #12495, #6933, #18339 ) ;
#18761 = DIRECTION ( 'NONE',  ( -0.9876526153536341335, -0.1566598588826327021, 0.000000000000000000 ) ) ;
#18762 = ORIENTED_EDGE ( 'NONE', *, *, #4042, .T. ) ;
#18763 = ORIENTED_EDGE ( 'NONE', *, *, #2209, .T. ) ;
#18764 = DIRECTION ( 'NONE',  ( 1.000000000000000000, 0.000000000000000000, 0.000000000000000000 ) ) ;
#18765 = DIRECTION ( 'NONE',  ( 0.000000000000000000, 0.000000000000000000, 1.000000000000000000 ) ) ;
#18766 = VECTOR ( 'NONE', #8183, 1000.000000000000000 ) ;
#18767 = ORIENTED_EDGE ( 'NONE', *, *, #14249, .F. ) ;
#18768 = CARTESIAN_POINT ( 'NONE',  ( -28.26947477390680774, -24.73384407370567217, 17.32050807568881723 ) ) ;
#18769 = CIRCLE ( 'NONE', #17530, 1.500000000000000444 ) ;
#18770 = AXIS2_PLACEMENT_3D ( 'NONE', #792, #9708, #5428 ) ;
#18771 = CARTESIAN_POINT ( 'NONE',  ( -33.00338452973448966, -20.42222043246805185, -21.65063509461098334 ) ) ;
#18772 = AXIS2_PLACEMENT_3D ( 'NONE', #13611, #7473, #14759 ) ;
#18773 = CARTESIAN_POINT ( 'NONE',  ( -25.76070822534488869, -82.04137586284720385, -17.32050807568878525 ) ) ;
#18774 = ADVANCED_FACE ( 'NONE', ( #4973 ), #4895, .F. ) ;
#18775 = DIRECTION ( 'NONE',  ( -0.1566598588826321192, 0.9876526153536342445, 7.798540720466731404E-17 ) ) ;
#18776 = CLOSED_SHELL ( 'NONE', ( #17490, #7583, #9445, #18752, #6197, #3988, #9617, #14270, #9348, #11409, #12640, #13770, #17735, #11330, #10080, #9244, #6557, #16498, #1527, #13594, #12769, #7422, #7545, #18598, #5695, #2172, #14946, #10964, #2691, #13021, #15417, #552, #1220, #8864, #9584, #15885, #7329, #7890, #13458, #17991, #2574, #5324, #4515, #11386, #15278, #2687, #4811, #9469 ) ) ;
#18777 = FACE_OUTER_BOUND ( 'NONE', #4476, .T. ) ;
#18779 = DIRECTION ( 'NONE',  ( -0.1566598588826321192, 0.9876526153536342445, 7.798540720466731404E-17 ) ) ;
#18778 = AXIS2_PLACEMENT_3D ( 'NONE', #10061, #5825, #11565 ) ;
#18780 = EDGE_CURVE ( 'NONE', #16318, #14250, #6628, .T. ) ;
#18781 = FACE_OUTER_BOUND ( 'NONE', #15437, .T. ) ;
#18782 = AXIS2_PLACEMENT_3D ( 'NONE', #372, #11706, #10309 ) ;
#18783 = ORIENTED_EDGE ( 'NONE', *, *, #14564, .F. ) ;
#18784 = DIRECTION ( 'NONE',  ( 3.039628882124824168E-17, 0.000000000000000000, -1.000000000000000000 ) ) ;
#18785 = EDGE_CURVE ( 'NONE', #2879, #13088, #7746, .T. ) ;
#18786 = EDGE_LOOP ( 'NONE', ( #5644, #409, #4098, #12793 ) ) ;
#18787 = CARTESIAN_POINT ( 'NONE',  ( -306.0881213225399051, -2.850701963179326448, -15.83618137761393463 ) ) ;
#18788 = ORIENTED_EDGE ( 'NONE', *, *, #6249, .F. ) ;
#18789 = ORIENTED_EDGE ( 'NONE', *, *, #4744, .T. ) ;
#18790 = VECTOR ( 'NONE', #7320, 1000.000000000000000 ) ;
#18791 = VECTOR ( 'NONE', #9207, 1000.000000000000000 ) ;
#18792 = CARTESIAN_POINT ( 'NONE',  ( 3.231158466157545206, -19.73726462726228092, 30.00000000000000000 ) ) ;
#18793 = ORIENTED_EDGE ( 'NONE', *, *, #2850, .T. ) ;
#18794 = EDGE_CURVE ( 'NONE', #5711, #4998, #12641, .T. ) ;
#18795 = NEXT_ASSEMBLY_USAGE_OCCURRENCE ( 'NAUO1', ' ', ' ', #1533, #8012, $ ) ;
#18796 = NEXT_ASSEMBLY_USAGE_OCCURRENCE ( 'NAUO2', ' ', ' ', #1533, #16949, $ ) ;
#18797 = NEXT_ASSEMBLY_USAGE_OCCURRENCE ( 'NAUO3', ' ', ' ', #1533, #9414, $ ) ;
#18798 = NEXT_ASSEMBLY_USAGE_OCCURRENCE ( 'NAUO4', ' ', ' ', #1533, #12169, $ ) ;
#18799 = NEXT_ASSEMBLY_USAGE_OCCURRENCE ( 'NAUO5', ' ', ' ', #1533, #12765, $ ) ;
#18800 = NEXT_ASSEMBLY_USAGE_OCCURRENCE ( 'NAUO6', ' ', ' ', #1533, #2110, $ ) ;
#18801 = NEXT_ASSEMBLY_USAGE_OCCURRENCE ( 'NAUO7', ' ', ' ', #1533, #12169, $ ) ;
#18802 = NEXT_ASSEMBLY_USAGE_OCCURRENCE ( 'NAUO8', ' ', ' ', #1533, #11363, $ ) ;
ENDSEC;
END-ISO-10303-21;
